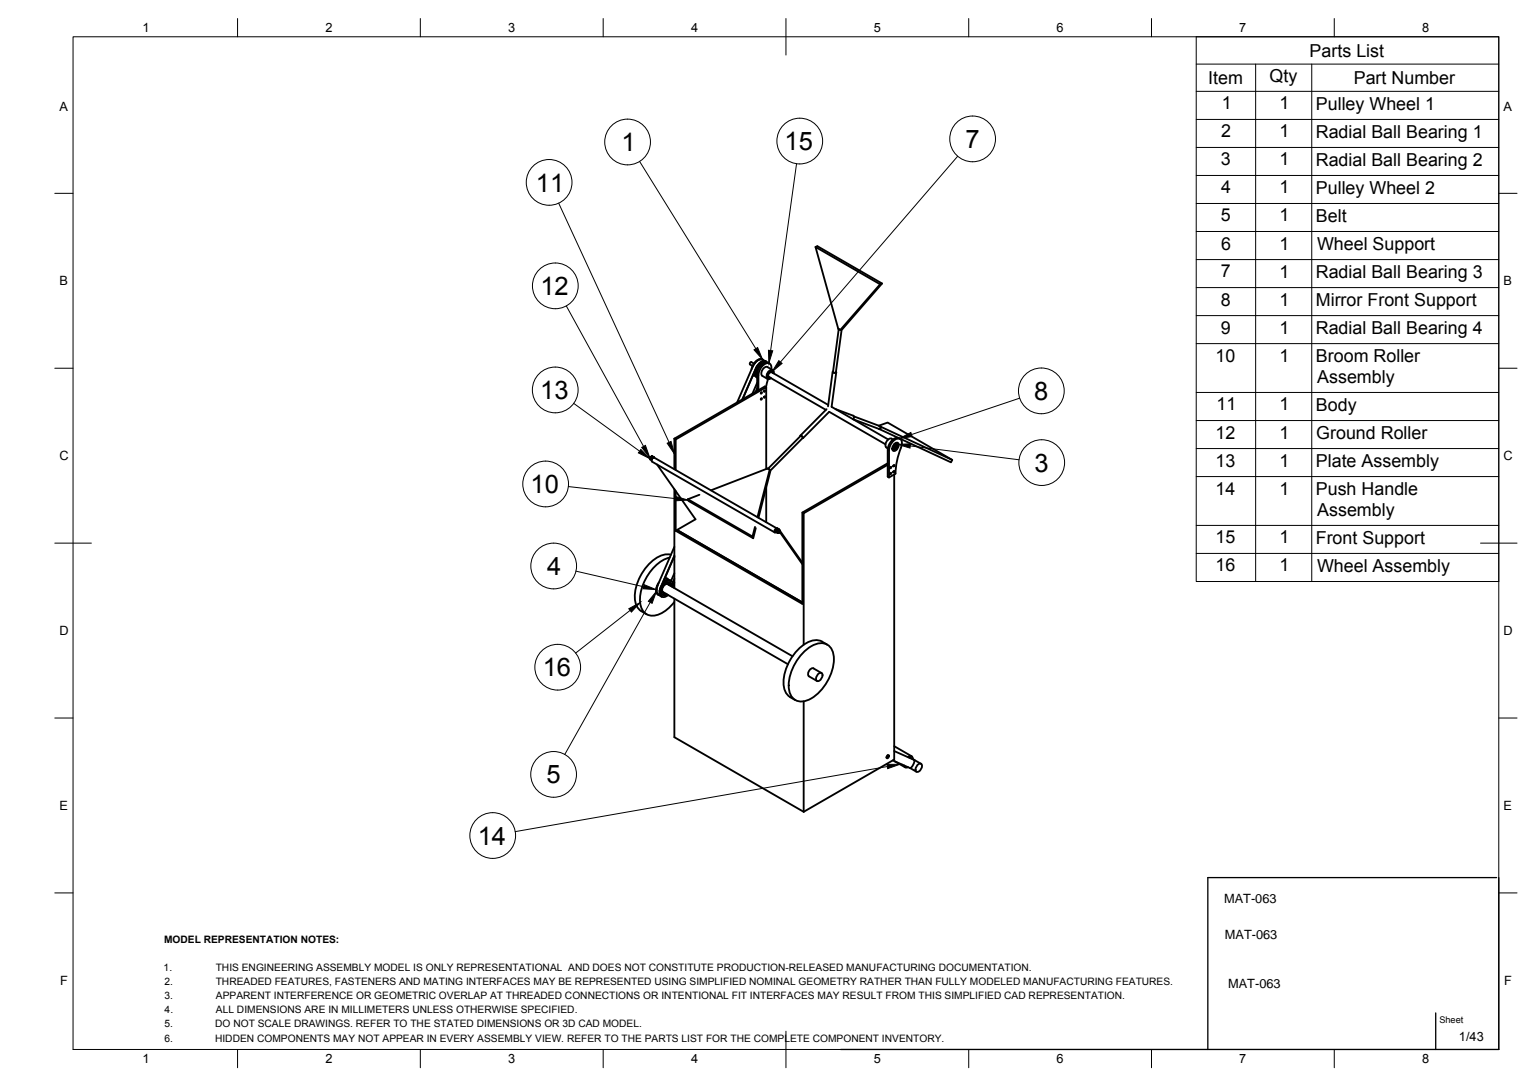
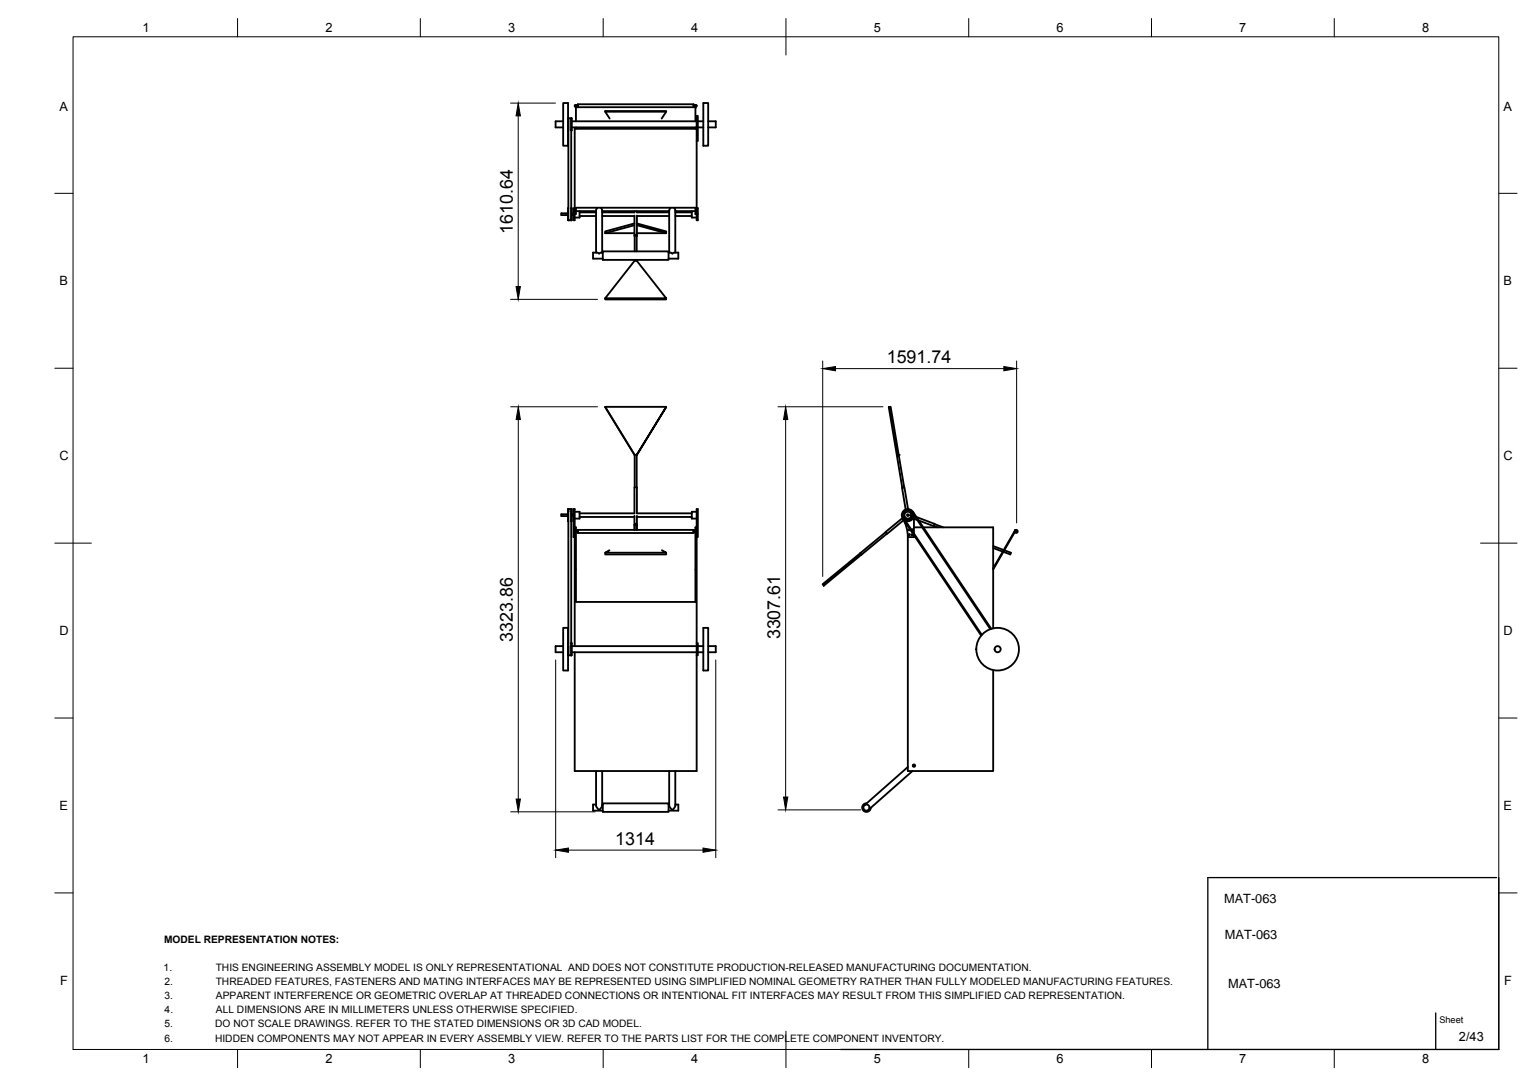
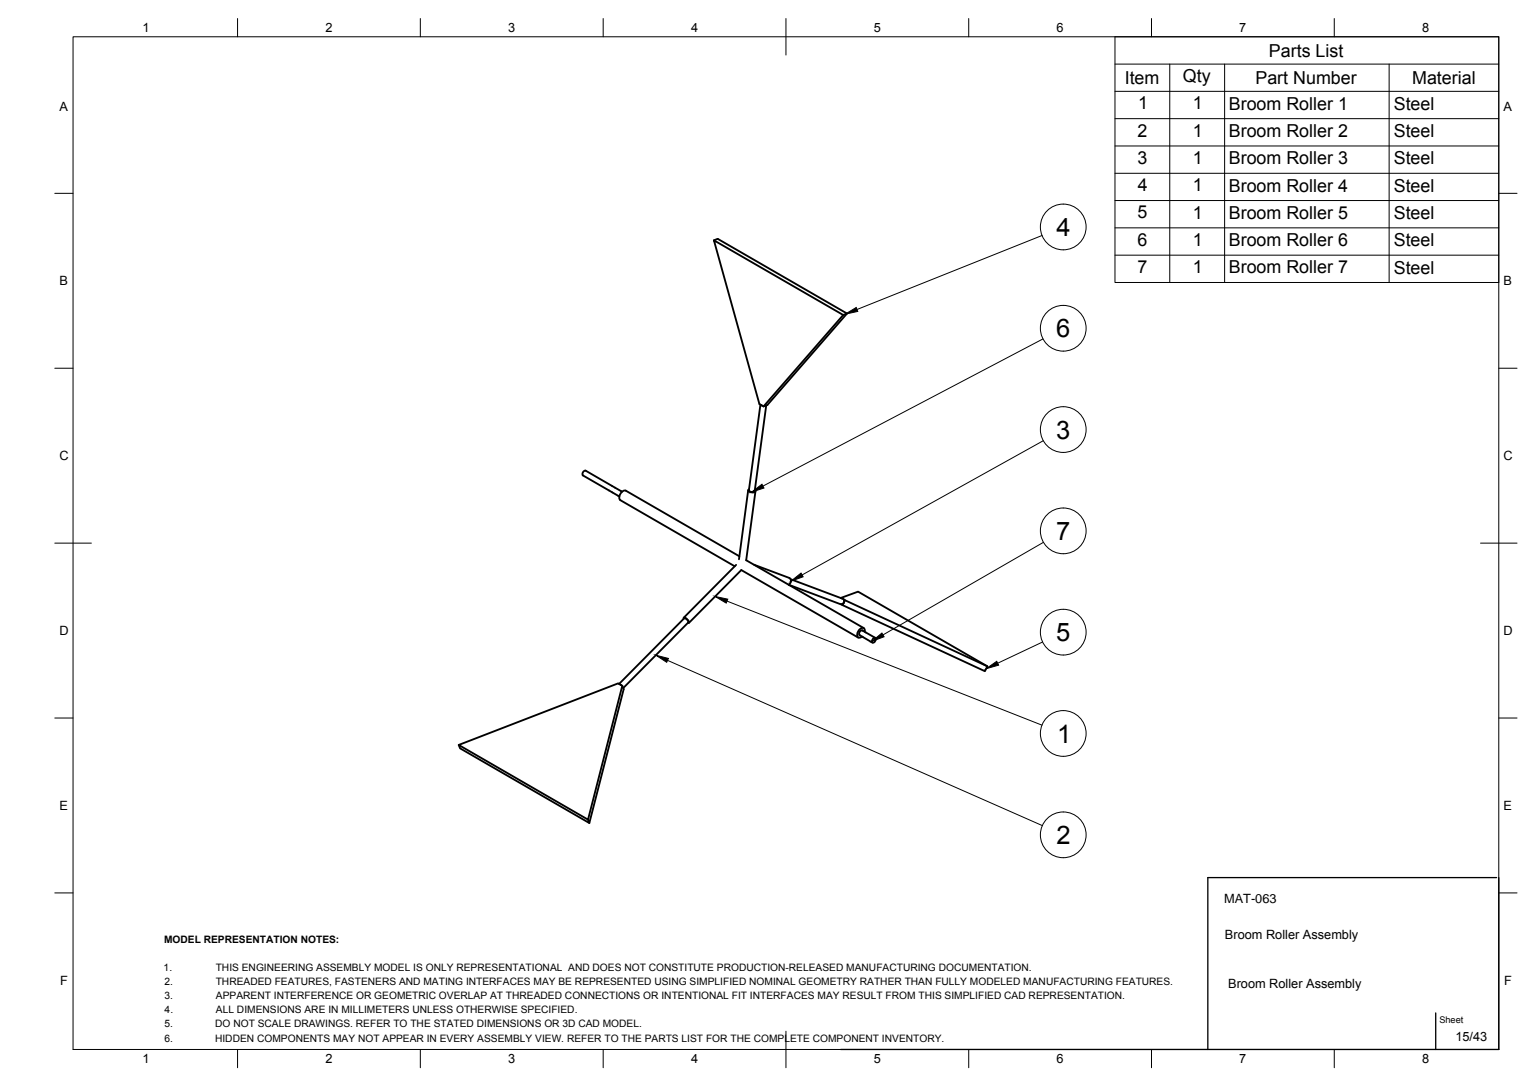
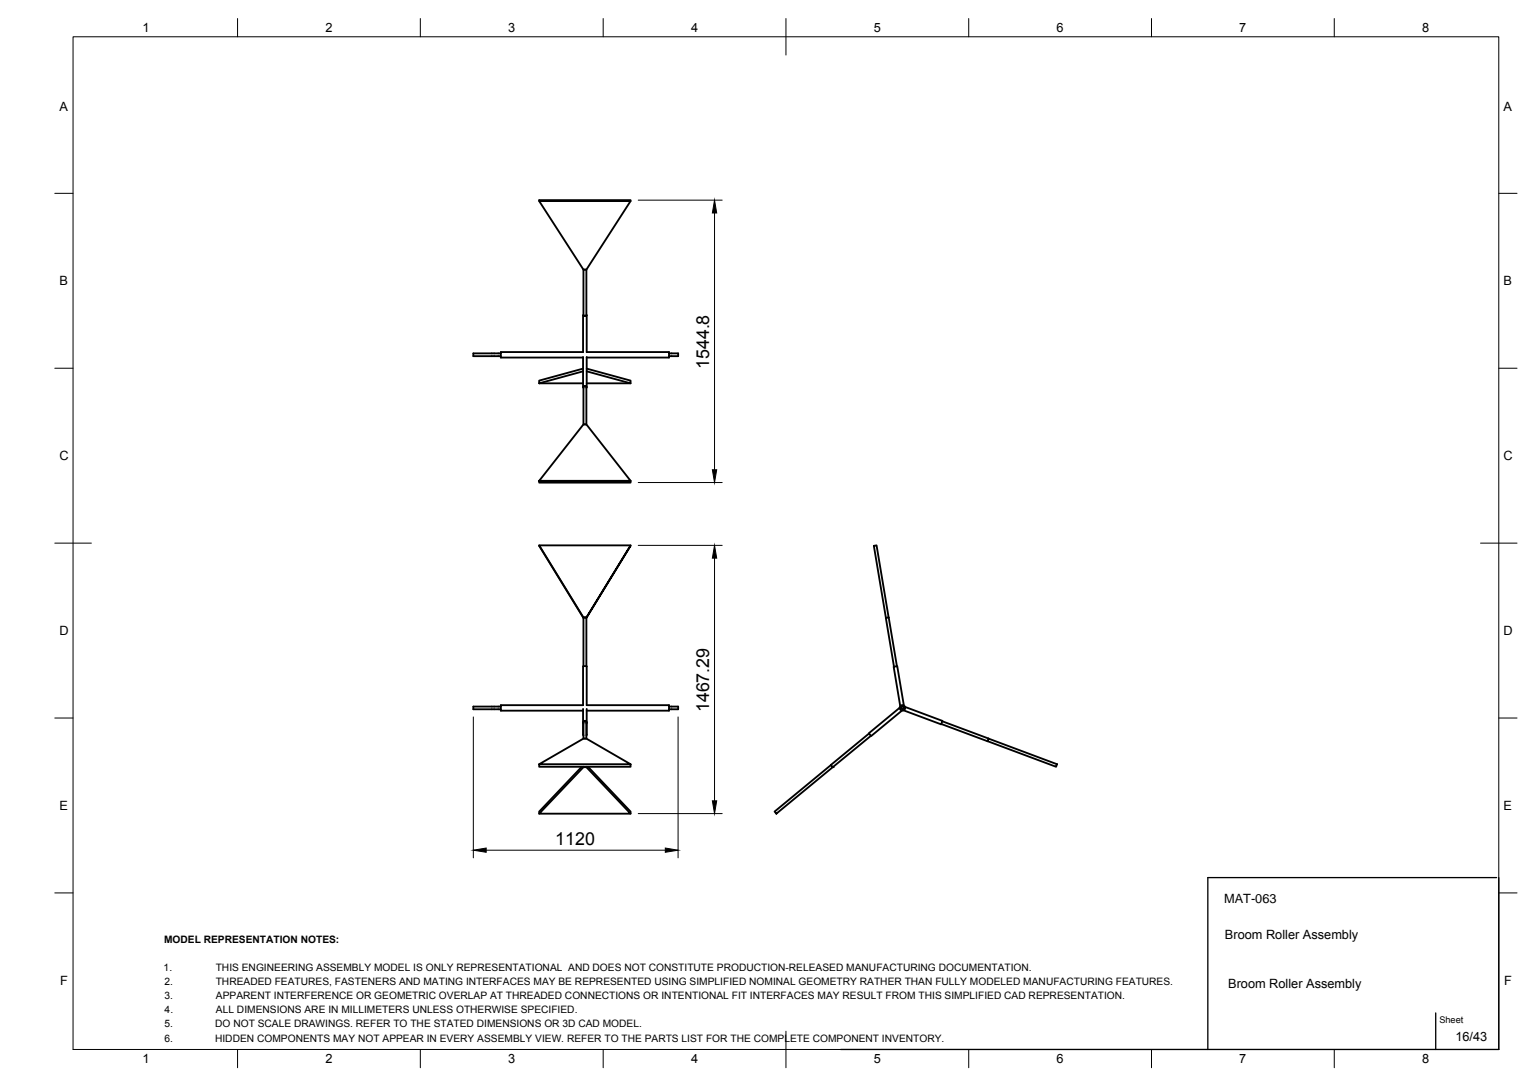
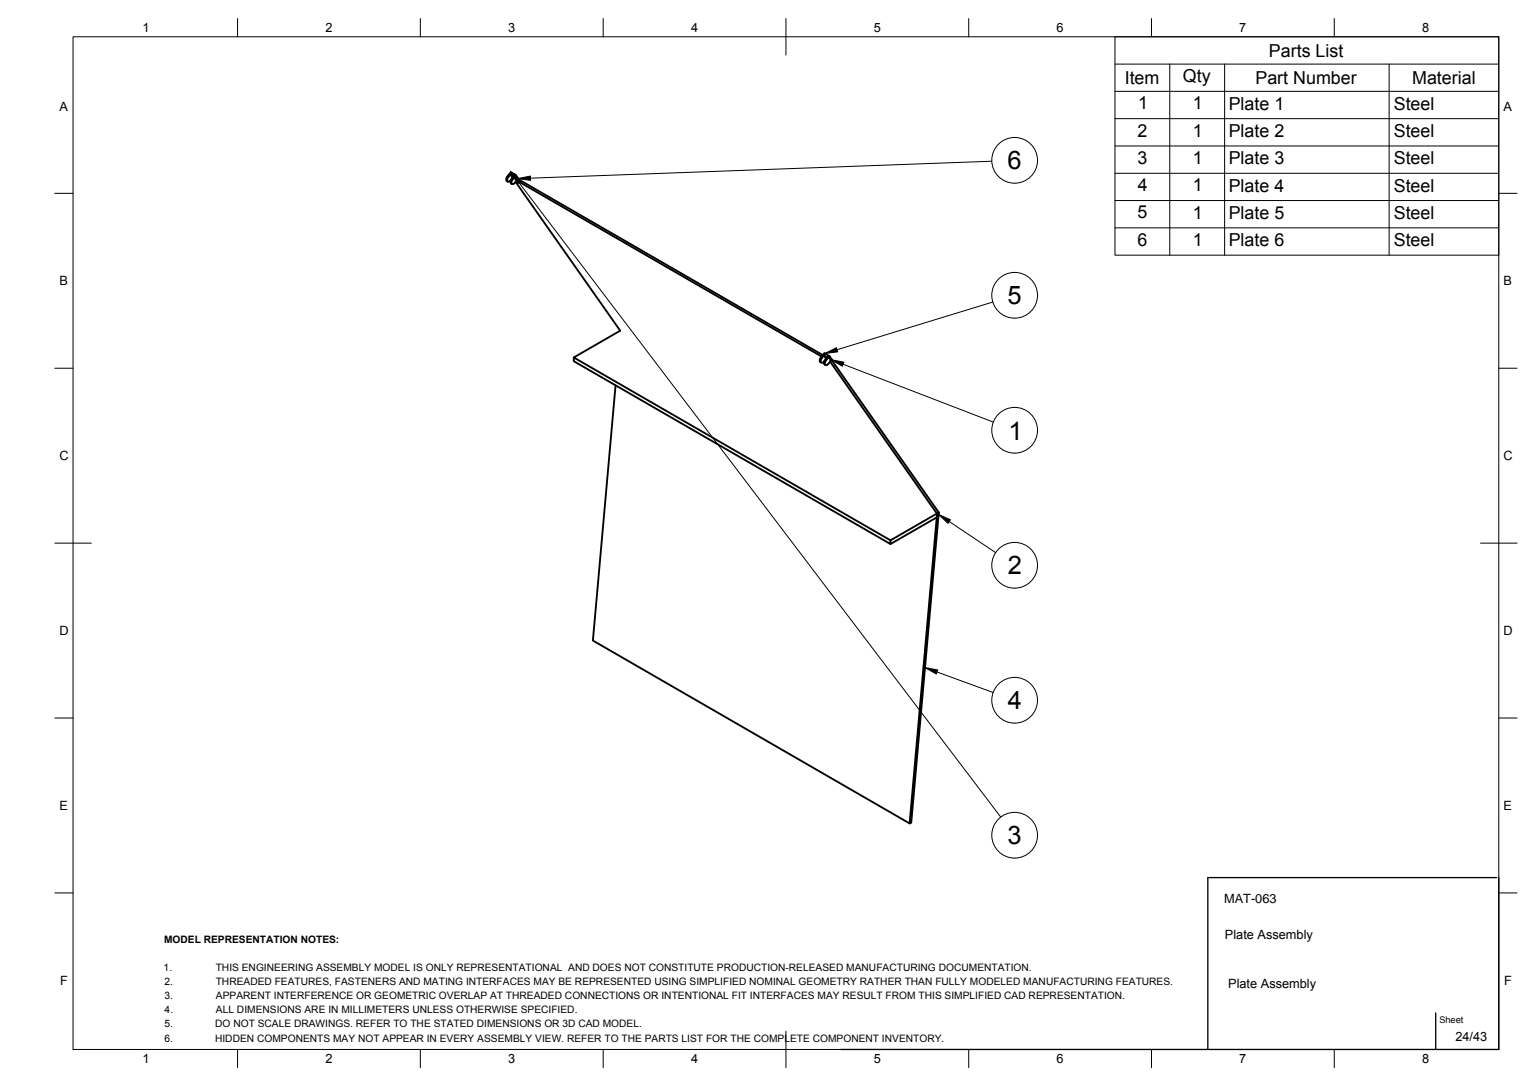
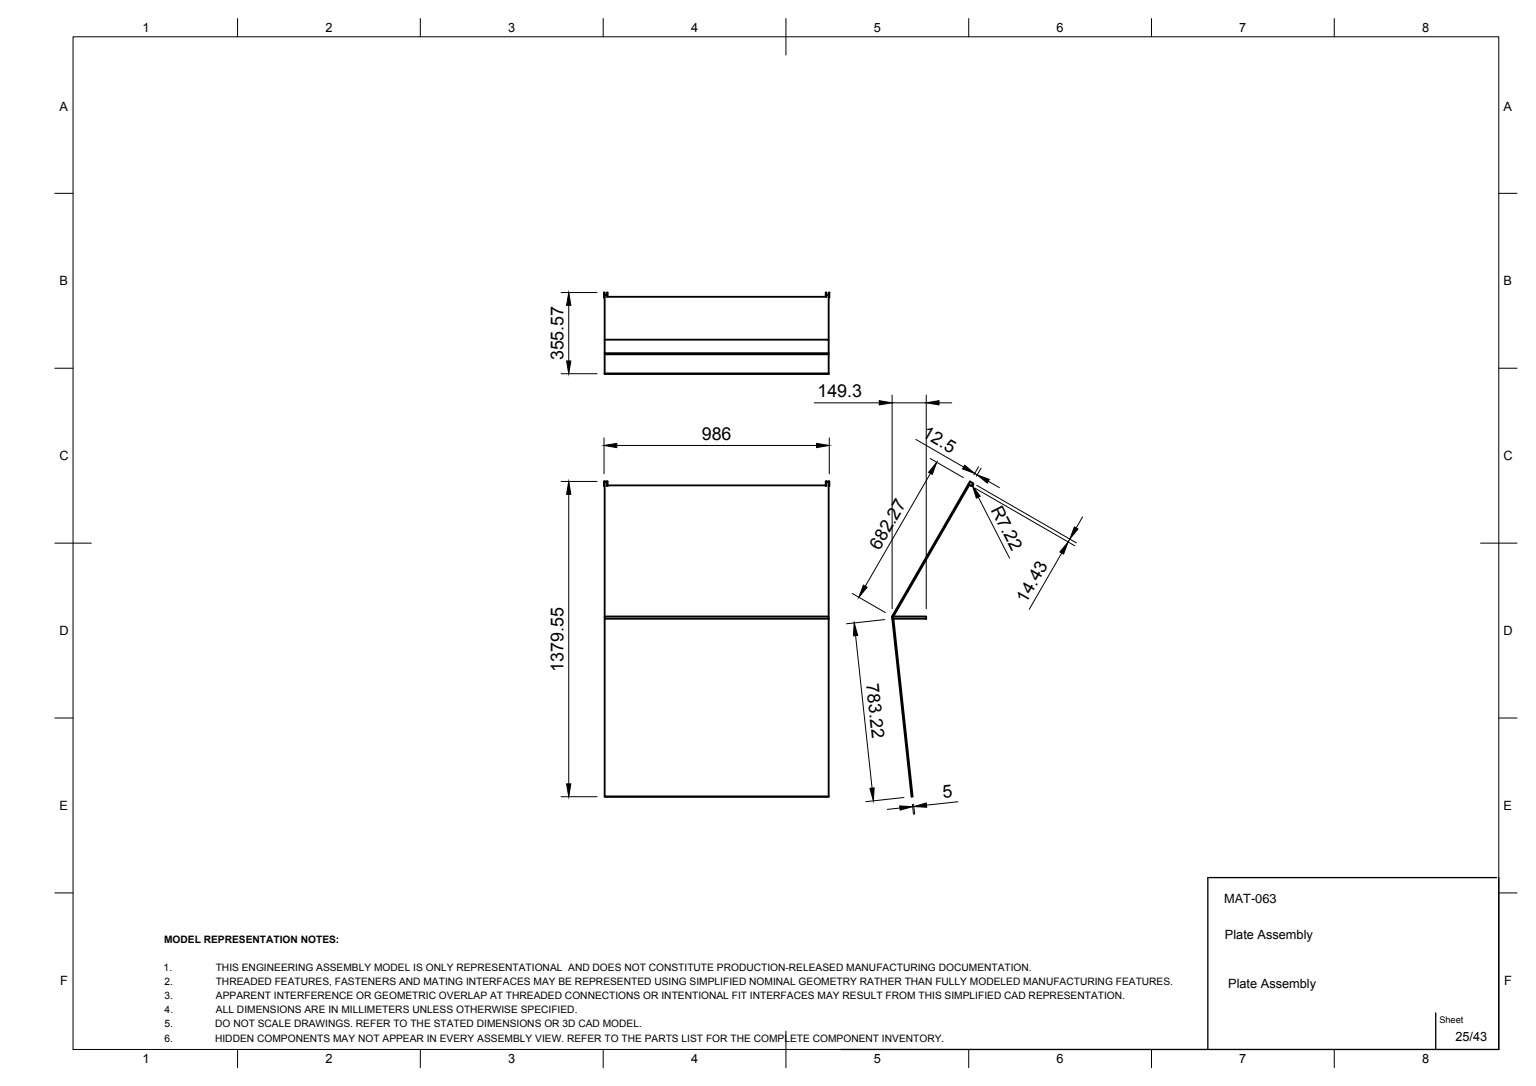
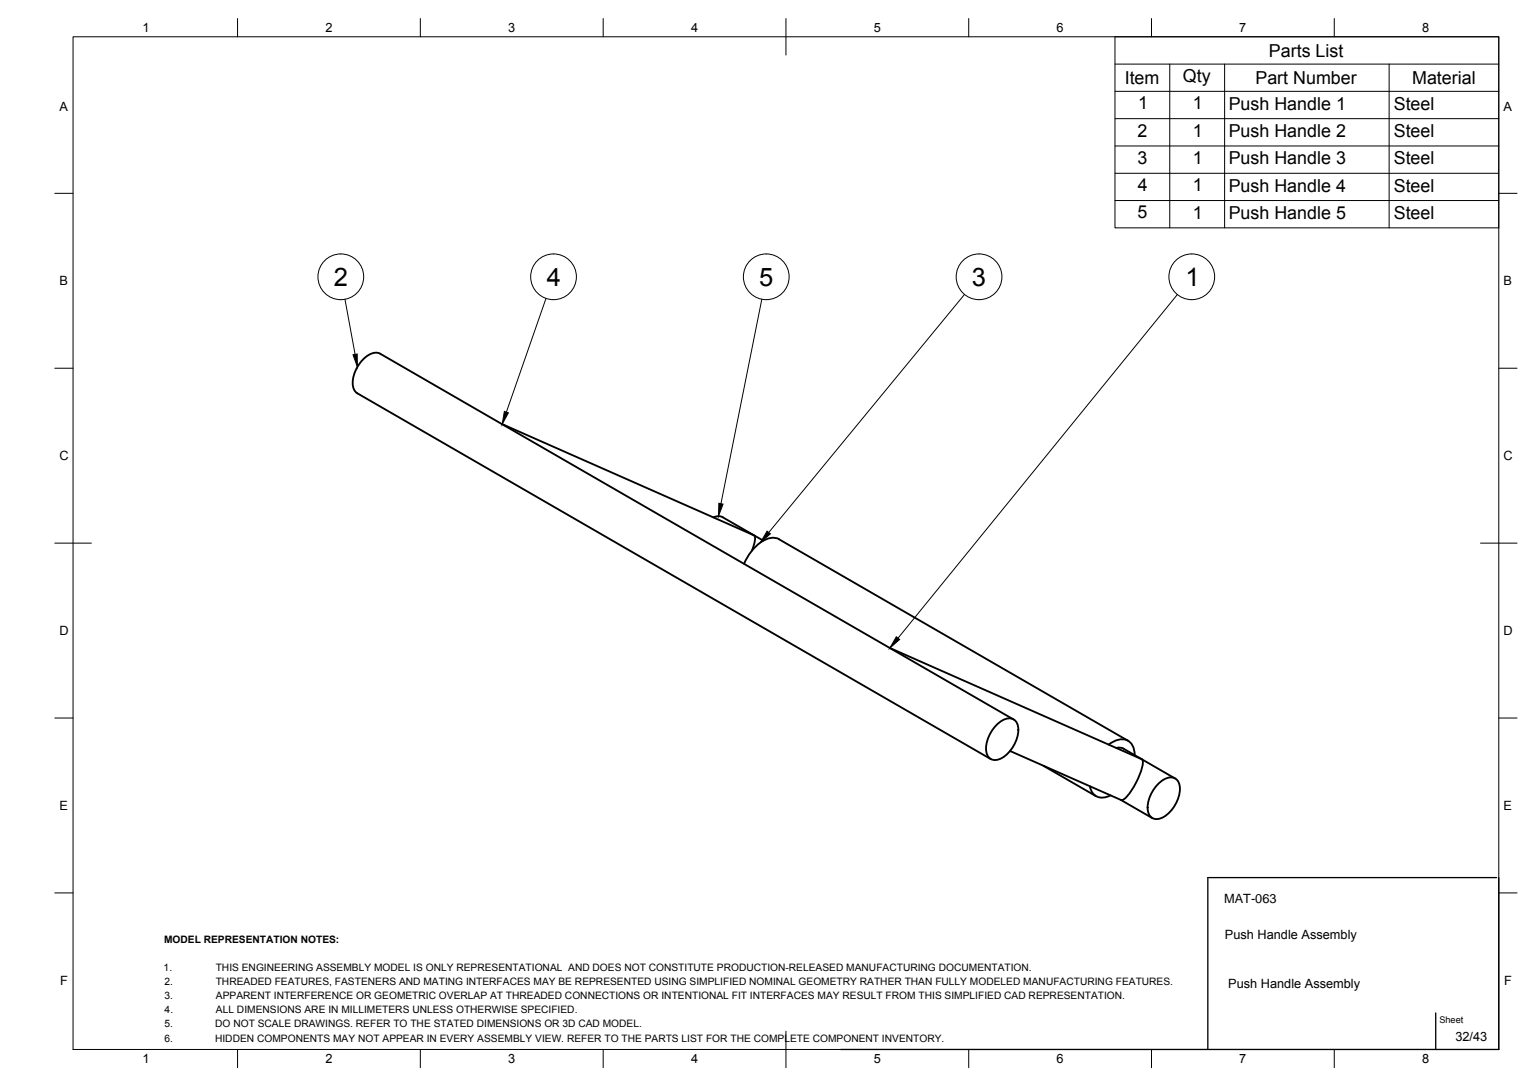
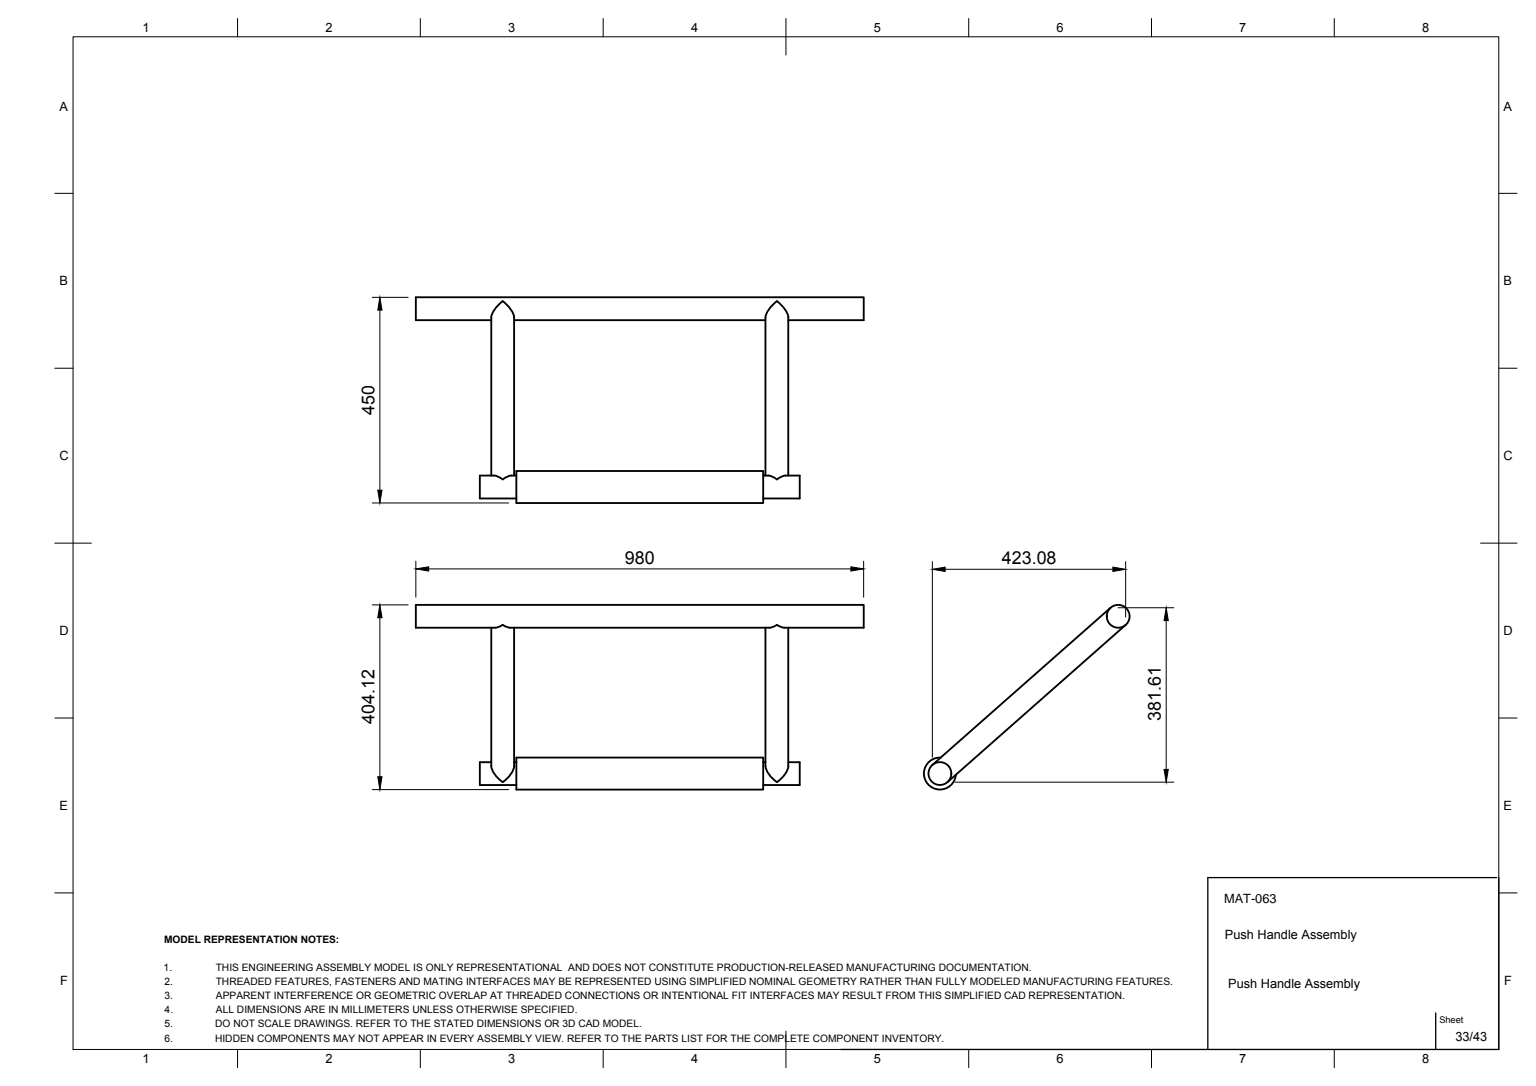
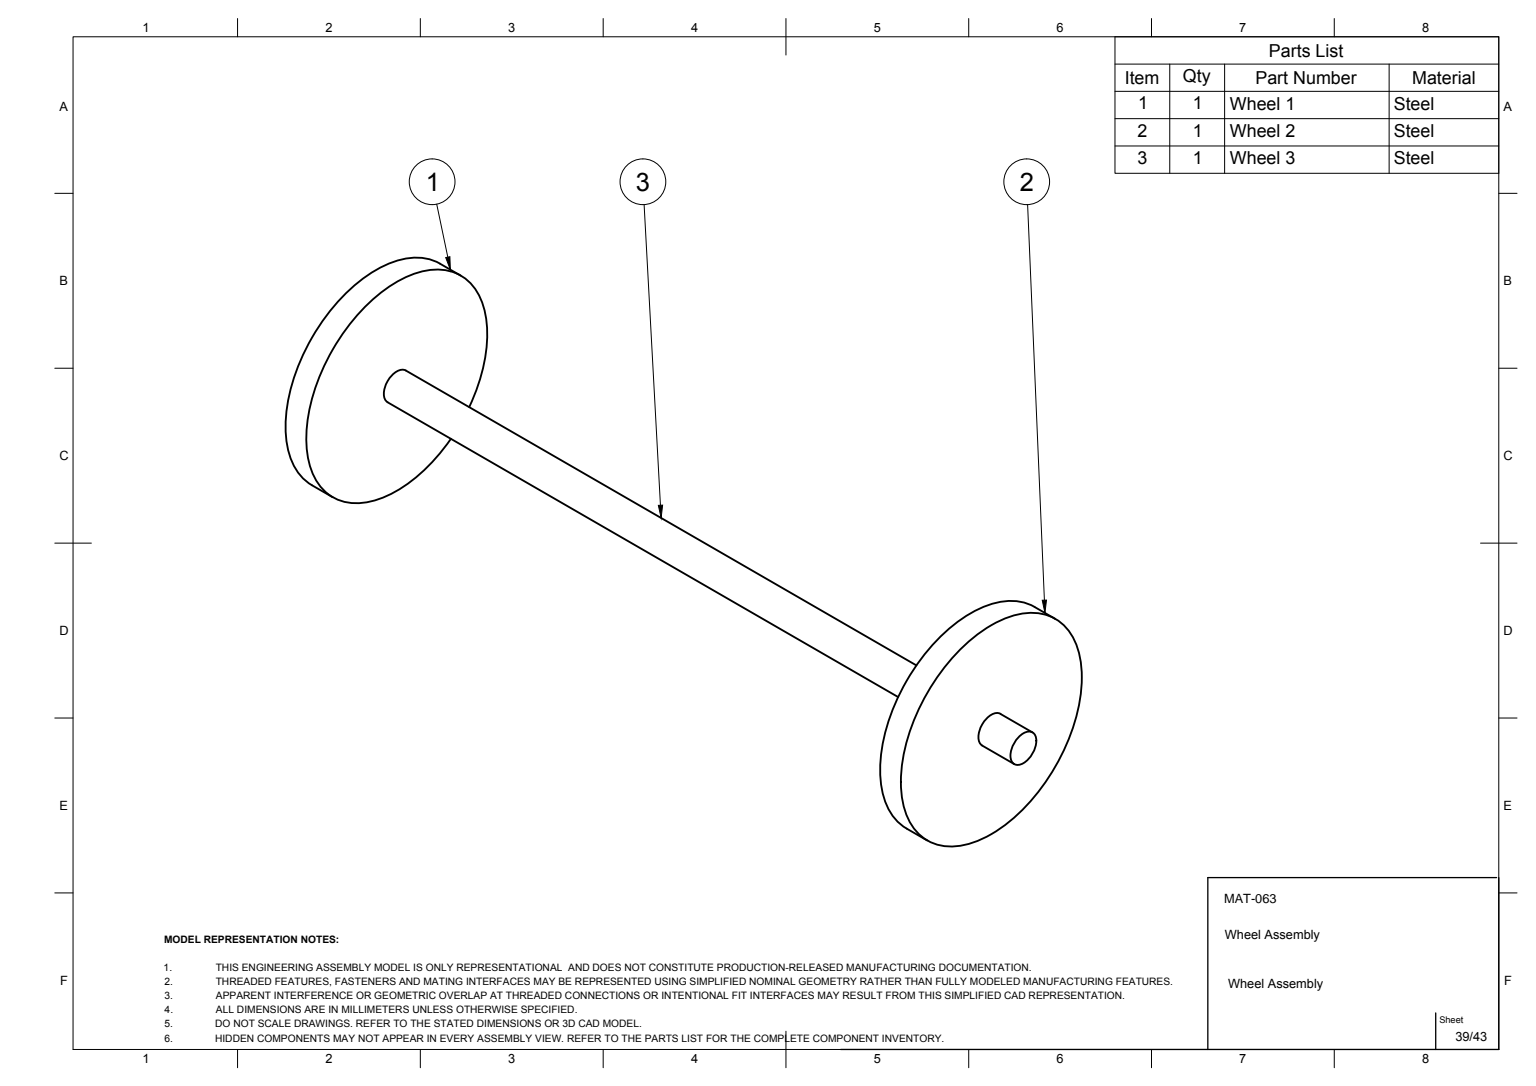
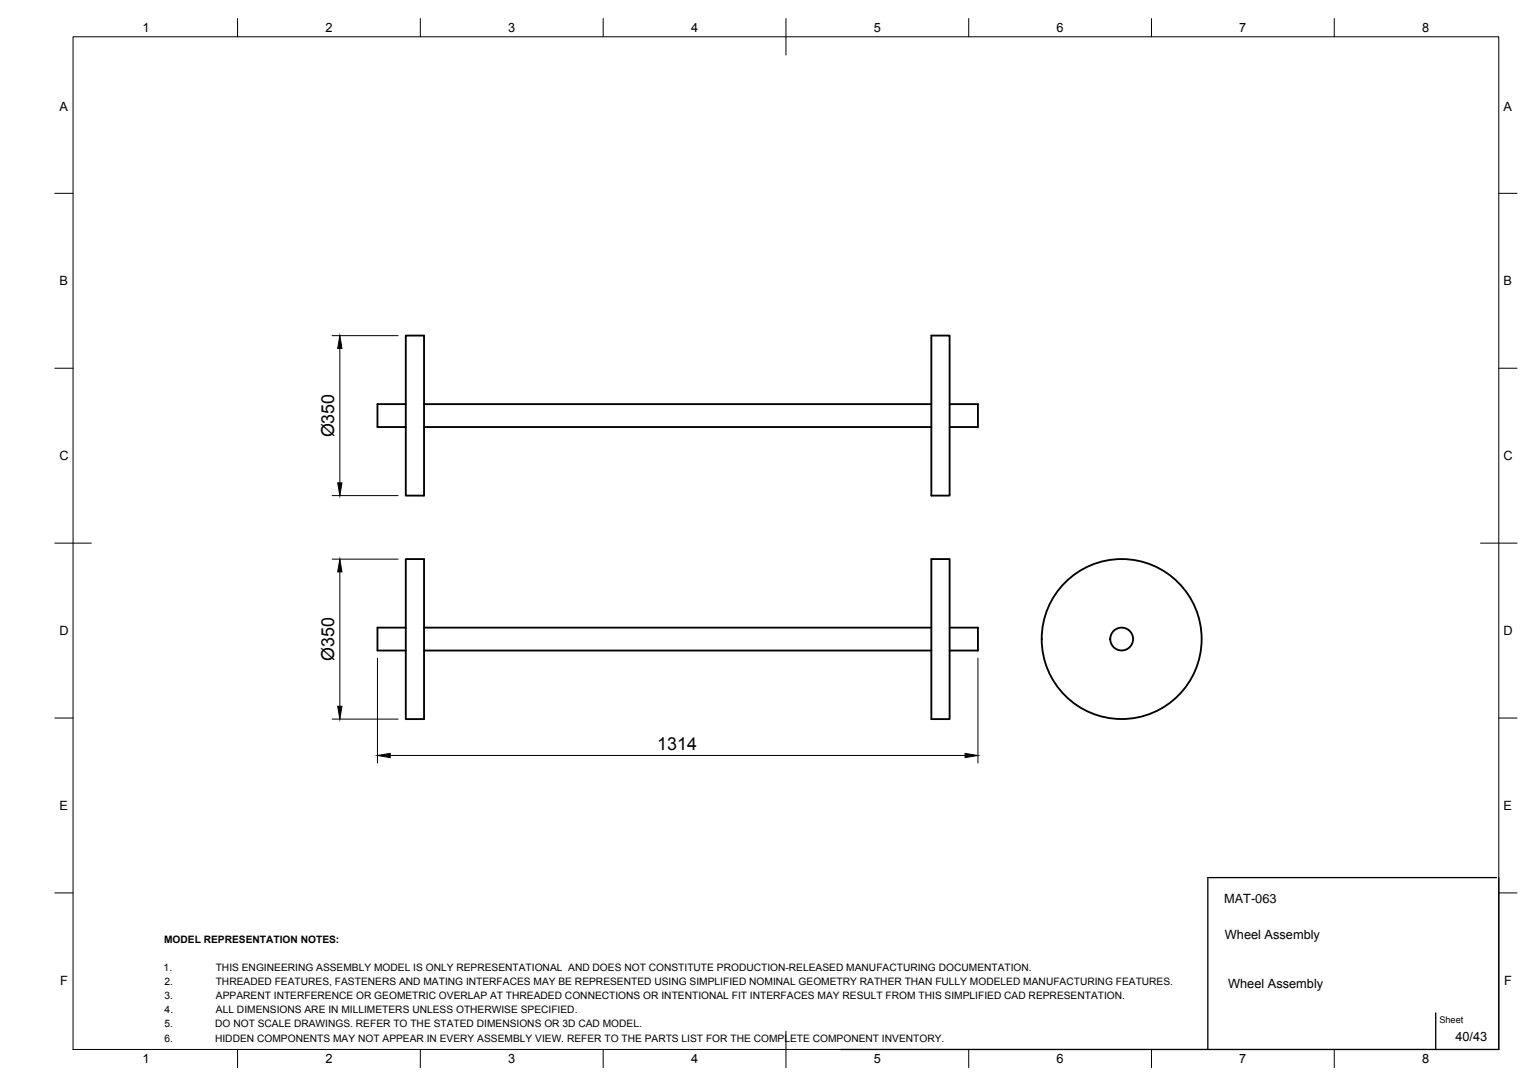
ISO-10303-21;
HEADER;
/* Generated by software containing ST-Developer
 * from STEP Tools, Inc. (www.steptools.com) 
 */

FILE_DESCRIPTION(
/* description */ (''),
/* implementation_level */ '2;1');

FILE_NAME(
/* name */ 'MAT-063',
/* time_stamp */ '2026-10-24T09:43:01-07:00',
/* author */ (''),
/* organization */ (''),
/* preprocessor_version */ 'ST-DEVELOPER v20.2',
/* originating_system */ 'Autodesk Translation Framework v15.15.0.0',
/* authorisation */ '');

FILE_SCHEMA (('AUTOMOTIVE_DESIGN { 1 0 10303 214 3 1 1 }'));
ENDSEC;

DATA;
#10=MECHANICAL_DESIGN_GEOMETRIC_PRESENTATION_REPRESENTATION('',(#273,#274,
#275,#276,#277,#278,#279,#280,#281,#282,#283,#284,#285,#286,#287,#288,#289,
#290,#291,#292,#293,#294,#295,#296,#297,#298,#299,#300,#301,#302,#303,#304,
#305),#11112);
#11=ELLIPSE('',#7146,0.035355338987388,0.0249999999491312);
#12=ELLIPSE('',#7147,0.0353553389873879,0.0249999999491312);
#13=ELLIPSE('',#7149,0.0353553389873867,0.0249999999491303);
#14=ELLIPSE('',#7150,0.0353553389873867,0.0249999999491303);
#15=ELLIPSE('',#7169,0.035355338987388,0.0249999999491312);
#16=ELLIPSE('',#7170,0.0353553389873879,0.0249999999491312);
#17=ELLIPSE('',#7172,0.0353553389873867,0.0249999999491303);
#18=ELLIPSE('',#7173,0.0353553389873867,0.0249999999491303);
#19=ITEM_DEFINED_TRANSFORMATION($,$,#6828,#6954);
#20=ITEM_DEFINED_TRANSFORMATION($,$,#6838,#6955);
#21=ITEM_DEFINED_TRANSFORMATION($,$,#6860,#6956);
#22=ITEM_DEFINED_TRANSFORMATION($,$,#6870,#6957);
#23=ITEM_DEFINED_TRANSFORMATION($,$,#6892,#6958);
#24=ITEM_DEFINED_TRANSFORMATION($,$,#6914,#6959);
#25=ITEM_DEFINED_TRANSFORMATION($,$,#6924,#6960);
#26=ITEM_DEFINED_TRANSFORMATION($,$,#7045,#7137);
#27=ITEM_DEFINED_TRANSFORMATION($,$,#7060,#7138);
#28=ITEM_DEFINED_TRANSFORMATION($,$,#7067,#7139);
#29=ITEM_DEFINED_TRANSFORMATION($,$,#7082,#7140);
#30=ITEM_DEFINED_TRANSFORMATION($,$,#7107,#7141);
#31=ITEM_DEFINED_TRANSFORMATION($,$,#7122,#7142);
#32=ITEM_DEFINED_TRANSFORMATION($,$,#7144,#7181);
#33=ITEM_DEFINED_TRANSFORMATION($,$,#7152,#7182);
#34=ITEM_DEFINED_TRANSFORMATION($,$,#7158,#7183);
#35=ITEM_DEFINED_TRANSFORMATION($,$,#7167,#7184);
#36=ITEM_DEFINED_TRANSFORMATION($,$,#7175,#7185);
#37=ITEM_DEFINED_TRANSFORMATION($,$,#7217,#7241);
#38=ITEM_DEFINED_TRANSFORMATION($,$,#7226,#7242);
#39=ITEM_DEFINED_TRANSFORMATION($,$,#7235,#7243);
#40=ITEM_DEFINED_TRANSFORMATION($,$,#6408,#7244);
#41=ITEM_DEFINED_TRANSFORMATION($,$,#6461,#7245);
#42=ITEM_DEFINED_TRANSFORMATION($,$,#6520,#7246);
#43=ITEM_DEFINED_TRANSFORMATION($,$,#6579,#7247);
#44=ITEM_DEFINED_TRANSFORMATION($,$,#6632,#7248);
#45=ITEM_DEFINED_TRANSFORMATION($,$,#6657,#7249);
#46=ITEM_DEFINED_TRANSFORMATION($,$,#6679,#7250);
#47=ITEM_DEFINED_TRANSFORMATION($,$,#6738,#7251);
#48=ITEM_DEFINED_TRANSFORMATION($,$,#6768,#7252);
#49=ITEM_DEFINED_TRANSFORMATION($,$,#6827,#7253);
#50=ITEM_DEFINED_TRANSFORMATION($,$,#6961,#7254);
#51=ITEM_DEFINED_TRANSFORMATION($,$,#7030,#7255);
#52=ITEM_DEFINED_TRANSFORMATION($,$,#7044,#7256);
#53=ITEM_DEFINED_TRANSFORMATION($,$,#7143,#7257);
#54=ITEM_DEFINED_TRANSFORMATION($,$,#7186,#7258);
#55=ITEM_DEFINED_TRANSFORMATION($,$,#7216,#7259);
#56=(
REPRESENTATION_RELATIONSHIP($,$,#11240,#11239)
REPRESENTATION_RELATIONSHIP_WITH_TRANSFORMATION(#19)
SHAPE_REPRESENTATION_RELATIONSHIP()
);
#57=(
REPRESENTATION_RELATIONSHIP($,$,#11241,#11239)
REPRESENTATION_RELATIONSHIP_WITH_TRANSFORMATION(#20)
SHAPE_REPRESENTATION_RELATIONSHIP()
);
#58=(
REPRESENTATION_RELATIONSHIP($,$,#11242,#11239)
REPRESENTATION_RELATIONSHIP_WITH_TRANSFORMATION(#21)
SHAPE_REPRESENTATION_RELATIONSHIP()
);
#59=(
REPRESENTATION_RELATIONSHIP($,$,#11243,#11239)
REPRESENTATION_RELATIONSHIP_WITH_TRANSFORMATION(#22)
SHAPE_REPRESENTATION_RELATIONSHIP()
);
#60=(
REPRESENTATION_RELATIONSHIP($,$,#11244,#11239)
REPRESENTATION_RELATIONSHIP_WITH_TRANSFORMATION(#23)
SHAPE_REPRESENTATION_RELATIONSHIP()
);
#61=(
REPRESENTATION_RELATIONSHIP($,$,#11245,#11239)
REPRESENTATION_RELATIONSHIP_WITH_TRANSFORMATION(#24)
SHAPE_REPRESENTATION_RELATIONSHIP()
);
#62=(
REPRESENTATION_RELATIONSHIP($,$,#11246,#11239)
REPRESENTATION_RELATIONSHIP_WITH_TRANSFORMATION(#25)
SHAPE_REPRESENTATION_RELATIONSHIP()
);
#63=(
REPRESENTATION_RELATIONSHIP($,$,#11250,#11249)
REPRESENTATION_RELATIONSHIP_WITH_TRANSFORMATION(#26)
SHAPE_REPRESENTATION_RELATIONSHIP()
);
#64=(
REPRESENTATION_RELATIONSHIP($,$,#11251,#11249)
REPRESENTATION_RELATIONSHIP_WITH_TRANSFORMATION(#27)
SHAPE_REPRESENTATION_RELATIONSHIP()
);
#65=(
REPRESENTATION_RELATIONSHIP($,$,#11252,#11249)
REPRESENTATION_RELATIONSHIP_WITH_TRANSFORMATION(#28)
SHAPE_REPRESENTATION_RELATIONSHIP()
);
#66=(
REPRESENTATION_RELATIONSHIP($,$,#11253,#11249)
REPRESENTATION_RELATIONSHIP_WITH_TRANSFORMATION(#29)
SHAPE_REPRESENTATION_RELATIONSHIP()
);
#67=(
REPRESENTATION_RELATIONSHIP($,$,#11254,#11249)
REPRESENTATION_RELATIONSHIP_WITH_TRANSFORMATION(#30)
SHAPE_REPRESENTATION_RELATIONSHIP()
);
#68=(
REPRESENTATION_RELATIONSHIP($,$,#11255,#11249)
REPRESENTATION_RELATIONSHIP_WITH_TRANSFORMATION(#31)
SHAPE_REPRESENTATION_RELATIONSHIP()
);
#69=(
REPRESENTATION_RELATIONSHIP($,$,#11257,#11256)
REPRESENTATION_RELATIONSHIP_WITH_TRANSFORMATION(#32)
SHAPE_REPRESENTATION_RELATIONSHIP()
);
#70=(
REPRESENTATION_RELATIONSHIP($,$,#11258,#11256)
REPRESENTATION_RELATIONSHIP_WITH_TRANSFORMATION(#33)
SHAPE_REPRESENTATION_RELATIONSHIP()
);
#71=(
REPRESENTATION_RELATIONSHIP($,$,#11259,#11256)
REPRESENTATION_RELATIONSHIP_WITH_TRANSFORMATION(#34)
SHAPE_REPRESENTATION_RELATIONSHIP()
);
#72=(
REPRESENTATION_RELATIONSHIP($,$,#11260,#11256)
REPRESENTATION_RELATIONSHIP_WITH_TRANSFORMATION(#35)
SHAPE_REPRESENTATION_RELATIONSHIP()
);
#73=(
REPRESENTATION_RELATIONSHIP($,$,#11261,#11256)
REPRESENTATION_RELATIONSHIP_WITH_TRANSFORMATION(#36)
SHAPE_REPRESENTATION_RELATIONSHIP()
);
#74=(
REPRESENTATION_RELATIONSHIP($,$,#11264,#11263)
REPRESENTATION_RELATIONSHIP_WITH_TRANSFORMATION(#37)
SHAPE_REPRESENTATION_RELATIONSHIP()
);
#75=(
REPRESENTATION_RELATIONSHIP($,$,#11265,#11263)
REPRESENTATION_RELATIONSHIP_WITH_TRANSFORMATION(#38)
SHAPE_REPRESENTATION_RELATIONSHIP()
);
#76=(
REPRESENTATION_RELATIONSHIP($,$,#11266,#11263)
REPRESENTATION_RELATIONSHIP_WITH_TRANSFORMATION(#39)
SHAPE_REPRESENTATION_RELATIONSHIP()
);
#77=(
REPRESENTATION_RELATIONSHIP($,$,#11230,#11229)
REPRESENTATION_RELATIONSHIP_WITH_TRANSFORMATION(#40)
SHAPE_REPRESENTATION_RELATIONSHIP()
);
#78=(
REPRESENTATION_RELATIONSHIP($,$,#11231,#11229)
REPRESENTATION_RELATIONSHIP_WITH_TRANSFORMATION(#41)
SHAPE_REPRESENTATION_RELATIONSHIP()
);
#79=(
REPRESENTATION_RELATIONSHIP($,$,#11232,#11229)
REPRESENTATION_RELATIONSHIP_WITH_TRANSFORMATION(#42)
SHAPE_REPRESENTATION_RELATIONSHIP()
);
#80=(
REPRESENTATION_RELATIONSHIP($,$,#11233,#11229)
REPRESENTATION_RELATIONSHIP_WITH_TRANSFORMATION(#43)
SHAPE_REPRESENTATION_RELATIONSHIP()
);
#81=(
REPRESENTATION_RELATIONSHIP($,$,#11234,#11229)
REPRESENTATION_RELATIONSHIP_WITH_TRANSFORMATION(#44)
SHAPE_REPRESENTATION_RELATIONSHIP()
);
#82=(
REPRESENTATION_RELATIONSHIP($,$,#11235,#11229)
REPRESENTATION_RELATIONSHIP_WITH_TRANSFORMATION(#45)
SHAPE_REPRESENTATION_RELATIONSHIP()
);
#83=(
REPRESENTATION_RELATIONSHIP($,$,#11236,#11229)
REPRESENTATION_RELATIONSHIP_WITH_TRANSFORMATION(#46)
SHAPE_REPRESENTATION_RELATIONSHIP()
);
#84=(
REPRESENTATION_RELATIONSHIP($,$,#11237,#11229)
REPRESENTATION_RELATIONSHIP_WITH_TRANSFORMATION(#47)
SHAPE_REPRESENTATION_RELATIONSHIP()
);
#85=(
REPRESENTATION_RELATIONSHIP($,$,#11238,#11229)
REPRESENTATION_RELATIONSHIP_WITH_TRANSFORMATION(#48)
SHAPE_REPRESENTATION_RELATIONSHIP()
);
#86=(
REPRESENTATION_RELATIONSHIP($,$,#11239,#11229)
REPRESENTATION_RELATIONSHIP_WITH_TRANSFORMATION(#49)
SHAPE_REPRESENTATION_RELATIONSHIP()
);
#87=(
REPRESENTATION_RELATIONSHIP($,$,#11247,#11229)
REPRESENTATION_RELATIONSHIP_WITH_TRANSFORMATION(#50)
SHAPE_REPRESENTATION_RELATIONSHIP()
);
#88=(
REPRESENTATION_RELATIONSHIP($,$,#11248,#11229)
REPRESENTATION_RELATIONSHIP_WITH_TRANSFORMATION(#51)
SHAPE_REPRESENTATION_RELATIONSHIP()
);
#89=(
REPRESENTATION_RELATIONSHIP($,$,#11249,#11229)
REPRESENTATION_RELATIONSHIP_WITH_TRANSFORMATION(#52)
SHAPE_REPRESENTATION_RELATIONSHIP()
);
#90=(
REPRESENTATION_RELATIONSHIP($,$,#11256,#11229)
REPRESENTATION_RELATIONSHIP_WITH_TRANSFORMATION(#53)
SHAPE_REPRESENTATION_RELATIONSHIP()
);
#91=(
REPRESENTATION_RELATIONSHIP($,$,#11262,#11229)
REPRESENTATION_RELATIONSHIP_WITH_TRANSFORMATION(#54)
SHAPE_REPRESENTATION_RELATIONSHIP()
);
#92=(
REPRESENTATION_RELATIONSHIP($,$,#11263,#11229)
REPRESENTATION_RELATIONSHIP_WITH_TRANSFORMATION(#55)
SHAPE_REPRESENTATION_RELATIONSHIP()
);
#93=CONTEXT_DEPENDENT_SHAPE_REPRESENTATION(#56,#11172);
#94=CONTEXT_DEPENDENT_SHAPE_REPRESENTATION(#57,#11173);
#95=CONTEXT_DEPENDENT_SHAPE_REPRESENTATION(#58,#11174);
#96=CONTEXT_DEPENDENT_SHAPE_REPRESENTATION(#59,#11175);
#97=CONTEXT_DEPENDENT_SHAPE_REPRESENTATION(#60,#11176);
#98=CONTEXT_DEPENDENT_SHAPE_REPRESENTATION(#61,#11177);
#99=CONTEXT_DEPENDENT_SHAPE_REPRESENTATION(#62,#11178);
#100=CONTEXT_DEPENDENT_SHAPE_REPRESENTATION(#63,#11188);
#101=CONTEXT_DEPENDENT_SHAPE_REPRESENTATION(#64,#11189);
#102=CONTEXT_DEPENDENT_SHAPE_REPRESENTATION(#65,#11190);
#103=CONTEXT_DEPENDENT_SHAPE_REPRESENTATION(#66,#11191);
#104=CONTEXT_DEPENDENT_SHAPE_REPRESENTATION(#67,#11192);
#105=CONTEXT_DEPENDENT_SHAPE_REPRESENTATION(#68,#11193);
#106=CONTEXT_DEPENDENT_SHAPE_REPRESENTATION(#69,#11200);
#107=CONTEXT_DEPENDENT_SHAPE_REPRESENTATION(#70,#11201);
#108=CONTEXT_DEPENDENT_SHAPE_REPRESENTATION(#71,#11202);
#109=CONTEXT_DEPENDENT_SHAPE_REPRESENTATION(#72,#11203);
#110=CONTEXT_DEPENDENT_SHAPE_REPRESENTATION(#73,#11204);
#111=CONTEXT_DEPENDENT_SHAPE_REPRESENTATION(#74,#11210);
#112=CONTEXT_DEPENDENT_SHAPE_REPRESENTATION(#75,#11211);
#113=CONTEXT_DEPENDENT_SHAPE_REPRESENTATION(#76,#11212);
#114=CONTEXT_DEPENDENT_SHAPE_REPRESENTATION(#77,#11213);
#115=CONTEXT_DEPENDENT_SHAPE_REPRESENTATION(#78,#11214);
#116=CONTEXT_DEPENDENT_SHAPE_REPRESENTATION(#79,#11215);
#117=CONTEXT_DEPENDENT_SHAPE_REPRESENTATION(#80,#11216);
#118=CONTEXT_DEPENDENT_SHAPE_REPRESENTATION(#81,#11217);
#119=CONTEXT_DEPENDENT_SHAPE_REPRESENTATION(#82,#11218);
#120=CONTEXT_DEPENDENT_SHAPE_REPRESENTATION(#83,#11219);
#121=CONTEXT_DEPENDENT_SHAPE_REPRESENTATION(#84,#11220);
#122=CONTEXT_DEPENDENT_SHAPE_REPRESENTATION(#85,#11221);
#123=CONTEXT_DEPENDENT_SHAPE_REPRESENTATION(#86,#11222);
#124=CONTEXT_DEPENDENT_SHAPE_REPRESENTATION(#87,#11223);
#125=CONTEXT_DEPENDENT_SHAPE_REPRESENTATION(#88,#11224);
#126=CONTEXT_DEPENDENT_SHAPE_REPRESENTATION(#89,#11225);
#127=CONTEXT_DEPENDENT_SHAPE_REPRESENTATION(#90,#11226);
#128=CONTEXT_DEPENDENT_SHAPE_REPRESENTATION(#91,#11227);
#129=CONTEXT_DEPENDENT_SHAPE_REPRESENTATION(#92,#11228);
#130=NEXT_ASSEMBLY_USAGE_OCCURRENCE('Broom Roller 1:1',
'Broom Roller 1:1','Broom Roller 1:1',#11278,#11279,'Broom Roller 1:1');
#131=NEXT_ASSEMBLY_USAGE_OCCURRENCE('Broom Roller 2:1',
'Broom Roller 2:1','Broom Roller 2:1',#11278,#11280,'Broom Roller 2:1');
#132=NEXT_ASSEMBLY_USAGE_OCCURRENCE('Broom Roller 3:1',
'Broom Roller 3:1','Broom Roller 3:1',#11278,#11281,'Broom Roller 3:1');
#133=NEXT_ASSEMBLY_USAGE_OCCURRENCE('Broom Roller 4:1',
'Broom Roller 4:1','Broom Roller 4:1',#11278,#11282,'Broom Roller 4:1');
#134=NEXT_ASSEMBLY_USAGE_OCCURRENCE('Broom Roller 5:1',
'Broom Roller 5:1','Broom Roller 5:1',#11278,#11283,'Broom Roller 5:1');
#135=NEXT_ASSEMBLY_USAGE_OCCURRENCE('Broom Roller 6:1',
'Broom Roller 6:1','Broom Roller 6:1',#11278,#11284,'Broom Roller 6:1');
#136=NEXT_ASSEMBLY_USAGE_OCCURRENCE('Broom Roller 7:1',
'Broom Roller 7:1','Broom Roller 7:1',#11278,#11285,'Broom Roller 7:1');
#137=NEXT_ASSEMBLY_USAGE_OCCURRENCE('Plate 1:1','Plate 1:1','Plate 1:1',
#11288,#11289,'Plate 1:1');
#138=NEXT_ASSEMBLY_USAGE_OCCURRENCE('Plate 2:1','Plate 2:1','Plate 2:1',
#11288,#11290,'Plate 2:1');
#139=NEXT_ASSEMBLY_USAGE_OCCURRENCE('Plate 3:1','Plate 3:1','Plate 3:1',
#11288,#11291,'Plate 3:1');
#140=NEXT_ASSEMBLY_USAGE_OCCURRENCE('Plate 4:1','Plate 4:1','Plate 4:1',
#11288,#11292,'Plate 4:1');
#141=NEXT_ASSEMBLY_USAGE_OCCURRENCE('Plate 5:1','Plate 5:1','Plate 5:1',
#11288,#11293,'Plate 5:1');
#142=NEXT_ASSEMBLY_USAGE_OCCURRENCE('Plate 6:1','Plate 6:1','Plate 6:1',
#11288,#11294,'Plate 6:1');
#143=NEXT_ASSEMBLY_USAGE_OCCURRENCE('Push Handle 1:1','Push Handle 1:1',
'Push Handle 1:1',#11295,#11296,'Push Handle 1:1');
#144=NEXT_ASSEMBLY_USAGE_OCCURRENCE('Push Handle 2:1','Push Handle 2:1',
'Push Handle 2:1',#11295,#11297,'Push Handle 2:1');
#145=NEXT_ASSEMBLY_USAGE_OCCURRENCE('Push Handle 3:1','Push Handle 3:1',
'Push Handle 3:1',#11295,#11298,'Push Handle 3:1');
#146=NEXT_ASSEMBLY_USAGE_OCCURRENCE('Push Handle 4:1','Push Handle 4:1',
'Push Handle 4:1',#11295,#11299,'Push Handle 4:1');
#147=NEXT_ASSEMBLY_USAGE_OCCURRENCE('Push Handle 5:1','Push Handle 5:1',
'Push Handle 5:1',#11295,#11300,'Push Handle 5:1');
#148=NEXT_ASSEMBLY_USAGE_OCCURRENCE('Wheel 1:1','Wheel 1:1','Wheel 1:1',
#11302,#11303,'Wheel 1:1');
#149=NEXT_ASSEMBLY_USAGE_OCCURRENCE('Wheel 2:1','Wheel 2:1','Wheel 2:1',
#11302,#11304,'Wheel 2:1');
#150=NEXT_ASSEMBLY_USAGE_OCCURRENCE('Wheel 3:1','Wheel 3:1','Wheel 3:1',
#11302,#11305,'Wheel 3:1');
#151=NEXT_ASSEMBLY_USAGE_OCCURRENCE('Pulley Wheel 1:1',
'Pulley Wheel 1:1','Pulley Wheel 1:1',#11268,#11269,'Pulley Wheel 1:1');
#152=NEXT_ASSEMBLY_USAGE_OCCURRENCE('Radial Ball Bearing 1:1',
'Radial Ball Bearing 1:1','Radial Ball Bearing 1:1',#11268,#11270,
'Radial Ball Bearing 1:1');
#153=NEXT_ASSEMBLY_USAGE_OCCURRENCE('Radial Ball Bearing 2:1',
'Radial Ball Bearing 2:1','Radial Ball Bearing 2:1',#11268,#11271,
'Radial Ball Bearing 2:1');
#154=NEXT_ASSEMBLY_USAGE_OCCURRENCE('Pulley Wheel 2:1',
'Pulley Wheel 2:1','Pulley Wheel 2:1',#11268,#11272,'Pulley Wheel 2:1');
#155=NEXT_ASSEMBLY_USAGE_OCCURRENCE('Belt:1','Belt:1','Belt:1',#11268,#11273,
'Belt:1');
#156=NEXT_ASSEMBLY_USAGE_OCCURRENCE('Wheel Support:1','Wheel Support:1',
'Wheel Support:1',#11268,#11274,'Wheel Support:1');
#157=NEXT_ASSEMBLY_USAGE_OCCURRENCE('Radial Ball Bearing 3:1',
'Radial Ball Bearing 3:1','Radial Ball Bearing 3:1',#11268,#11275,
'Radial Ball Bearing 3:1');
#158=NEXT_ASSEMBLY_USAGE_OCCURRENCE('Mirror Front Support:1',
'Mirror Front Support:1','Mirror Front Support:1',#11268,#11276,
'Mirror Front Support:1');
#159=NEXT_ASSEMBLY_USAGE_OCCURRENCE('Radial Ball Bearing 4:1',
'Radial Ball Bearing 4:1','Radial Ball Bearing 4:1',#11268,#11277,
'Radial Ball Bearing 4:1');
#160=NEXT_ASSEMBLY_USAGE_OCCURRENCE('Broom Roller Assembly:1',
'Broom Roller Assembly:1','Broom Roller Assembly:1',#11268,#11278,
'Broom Roller Assembly:1');
#161=NEXT_ASSEMBLY_USAGE_OCCURRENCE('Body:1','Body:1','Body:1',#11268,#11286,
'Body:1');
#162=NEXT_ASSEMBLY_USAGE_OCCURRENCE('Ground Roller:1','Ground Roller:1',
'Ground Roller:1',#11268,#11287,'Ground Roller:1');
#163=NEXT_ASSEMBLY_USAGE_OCCURRENCE('Plate Assembly:1',
'Plate Assembly:1','Plate Assembly:1',#11268,#11288,'Plate Assembly:1');
#164=NEXT_ASSEMBLY_USAGE_OCCURRENCE('Push Handle Assembly:1',
'Push Handle Assembly:1','Push Handle Assembly:1',#11268,#11295,
'Push Handle Assembly:1');
#165=NEXT_ASSEMBLY_USAGE_OCCURRENCE('Front Support:1','Front Support:1',
'Front Support:1',#11268,#11301,'Front Support:1');
#166=NEXT_ASSEMBLY_USAGE_OCCURRENCE('Wheel Assembly:1',
'Wheel Assembly:1','Wheel Assembly:1',#11268,#11302,'Wheel Assembly:1');
#167=TOROIDAL_SURFACE('',#6462,0.0248999989285722,0.00110000131901909);
#168=TOROIDAL_SURFACE('',#6467,0.0248999989285722,0.00110000131901909);
#169=TOROIDAL_SURFACE('',#6475,0.0248999989285722,0.00110000131901911);
#170=TOROIDAL_SURFACE('',#6482,0.0248999989285722,0.00110000131901911);
#171=TOROIDAL_SURFACE('',#6486,0.01675,0.00555000054498457);
#172=TOROIDAL_SURFACE('',#6495,0.01675,0.00555000054498457);
#173=TOROIDAL_SURFACE('',#6504,0.00860000107142784,0.00110000131901912);
#174=TOROIDAL_SURFACE('',#6508,0.00860000107142784,0.00110000131901912);
#175=TOROIDAL_SURFACE('',#6516,0.00860000107142785,0.00110000131901912);
#176=TOROIDAL_SURFACE('',#6519,0.00860000107142785,0.00110000131901912);
#177=TOROIDAL_SURFACE('',#6521,0.0248999989285722,0.00110000131901909);
#178=TOROIDAL_SURFACE('',#6526,0.0248999989285722,0.00110000131901909);
#179=TOROIDAL_SURFACE('',#6534,0.0248999989285722,0.00110000131901911);
#180=TOROIDAL_SURFACE('',#6541,0.0248999989285722,0.00110000131901911);
#181=TOROIDAL_SURFACE('',#6545,0.01675,0.00555000054498457);
#182=TOROIDAL_SURFACE('',#6554,0.01675,0.00555000054498457);
#183=TOROIDAL_SURFACE('',#6563,0.00860000107142784,0.00110000131901912);
#184=TOROIDAL_SURFACE('',#6567,0.00860000107142784,0.00110000131901912);
#185=TOROIDAL_SURFACE('',#6575,0.00860000107142785,0.00110000131901912);
#186=TOROIDAL_SURFACE('',#6578,0.00860000107142785,0.00110000131901912);
#187=TOROIDAL_SURFACE('',#6680,0.0248999989285722,0.00110000131901909);
#188=TOROIDAL_SURFACE('',#6685,0.0248999989285722,0.00110000131901909);
#189=TOROIDAL_SURFACE('',#6693,0.0248999989285722,0.00110000131901911);
#190=TOROIDAL_SURFACE('',#6700,0.0248999989285722,0.00110000131901911);
#191=TOROIDAL_SURFACE('',#6704,0.01675,0.00555000054498457);
#192=TOROIDAL_SURFACE('',#6713,0.01675,0.00555000054498457);
#193=TOROIDAL_SURFACE('',#6722,0.00860000107142784,0.00110000131901912);
#194=TOROIDAL_SURFACE('',#6726,0.00860000107142784,0.00110000131901912);
#195=TOROIDAL_SURFACE('',#6734,0.00860000107142785,0.00110000131901912);
#196=TOROIDAL_SURFACE('',#6737,0.00860000107142785,0.00110000131901912);
#197=TOROIDAL_SURFACE('',#6769,0.0248999989285722,0.00110000131901909);
#198=TOROIDAL_SURFACE('',#6774,0.0248999989285722,0.00110000131901909);
#199=TOROIDAL_SURFACE('',#6782,0.0248999989285722,0.00110000131901911);
#200=TOROIDAL_SURFACE('',#6789,0.0248999989285722,0.00110000131901911);
#201=TOROIDAL_SURFACE('',#6793,0.01675,0.00555000054498457);
#202=TOROIDAL_SURFACE('',#6802,0.01675,0.00555000054498457);
#203=TOROIDAL_SURFACE('',#6811,0.00860000107142784,0.00110000131901912);
#204=TOROIDAL_SURFACE('',#6815,0.00860000107142784,0.00110000131901912);
#205=TOROIDAL_SURFACE('',#6823,0.00860000107142785,0.00110000131901912);
#206=TOROIDAL_SURFACE('',#6826,0.00860000107142785,0.00110000131901912);
#207=SHAPE_REPRESENTATION_RELATIONSHIP('SRR','None',#11230,#240);
#208=SHAPE_REPRESENTATION_RELATIONSHIP('SRR','None',#11231,#241);
#209=SHAPE_REPRESENTATION_RELATIONSHIP('SRR','None',#11232,#242);
#210=SHAPE_REPRESENTATION_RELATIONSHIP('SRR','None',#11233,#243);
#211=SHAPE_REPRESENTATION_RELATIONSHIP('SRR','None',#11234,#244);
#212=SHAPE_REPRESENTATION_RELATIONSHIP('SRR','None',#11235,#245);
#213=SHAPE_REPRESENTATION_RELATIONSHIP('SRR','None',#11236,#246);
#214=SHAPE_REPRESENTATION_RELATIONSHIP('SRR','None',#11237,#247);
#215=SHAPE_REPRESENTATION_RELATIONSHIP('SRR','None',#11238,#248);
#216=SHAPE_REPRESENTATION_RELATIONSHIP('SRR','None',#11240,#249);
#217=SHAPE_REPRESENTATION_RELATIONSHIP('SRR','None',#11241,#250);
#218=SHAPE_REPRESENTATION_RELATIONSHIP('SRR','None',#11242,#251);
#219=SHAPE_REPRESENTATION_RELATIONSHIP('SRR','None',#11243,#252);
#220=SHAPE_REPRESENTATION_RELATIONSHIP('SRR','None',#11244,#253);
#221=SHAPE_REPRESENTATION_RELATIONSHIP('SRR','None',#11245,#254);
#222=SHAPE_REPRESENTATION_RELATIONSHIP('SRR','None',#11246,#255);
#223=SHAPE_REPRESENTATION_RELATIONSHIP('SRR','None',#11247,#256);
#224=SHAPE_REPRESENTATION_RELATIONSHIP('SRR','None',#11248,#257);
#225=SHAPE_REPRESENTATION_RELATIONSHIP('SRR','None',#11250,#258);
#226=SHAPE_REPRESENTATION_RELATIONSHIP('SRR','None',#11251,#259);
#227=SHAPE_REPRESENTATION_RELATIONSHIP('SRR','None',#11252,#260);
#228=SHAPE_REPRESENTATION_RELATIONSHIP('SRR','None',#11253,#261);
#229=SHAPE_REPRESENTATION_RELATIONSHIP('SRR','None',#11254,#262);
#230=SHAPE_REPRESENTATION_RELATIONSHIP('SRR','None',#11255,#263);
#231=SHAPE_REPRESENTATION_RELATIONSHIP('SRR','None',#11257,#264);
#232=SHAPE_REPRESENTATION_RELATIONSHIP('SRR','None',#11258,#265);
#233=SHAPE_REPRESENTATION_RELATIONSHIP('SRR','None',#11259,#266);
#234=SHAPE_REPRESENTATION_RELATIONSHIP('SRR','None',#11260,#267);
#235=SHAPE_REPRESENTATION_RELATIONSHIP('SRR','None',#11261,#268);
#236=SHAPE_REPRESENTATION_RELATIONSHIP('SRR','None',#11262,#269);
#237=SHAPE_REPRESENTATION_RELATIONSHIP('SRR','None',#11264,#270);
#238=SHAPE_REPRESENTATION_RELATIONSHIP('SRR','None',#11265,#271);
#239=SHAPE_REPRESENTATION_RELATIONSHIP('SRR','None',#11266,#272);
#240=ADVANCED_BREP_SHAPE_REPRESENTATION('',(#306),#11075);
#241=ADVANCED_BREP_SHAPE_REPRESENTATION('',(#307),#11076);
#242=ADVANCED_BREP_SHAPE_REPRESENTATION('',(#308),#11077);
#243=ADVANCED_BREP_SHAPE_REPRESENTATION('',(#309),#11078);
#244=ADVANCED_BREP_SHAPE_REPRESENTATION('',(#310),#11079);
#245=ADVANCED_BREP_SHAPE_REPRESENTATION('',(#311),#11080);
#246=ADVANCED_BREP_SHAPE_REPRESENTATION('',(#312),#11081);
#247=ADVANCED_BREP_SHAPE_REPRESENTATION('',(#313),#11082);
#248=ADVANCED_BREP_SHAPE_REPRESENTATION('',(#314),#11083);
#249=ADVANCED_BREP_SHAPE_REPRESENTATION('',(#315),#11085);
#250=ADVANCED_BREP_SHAPE_REPRESENTATION('',(#316),#11086);
#251=ADVANCED_BREP_SHAPE_REPRESENTATION('',(#317),#11087);
#252=ADVANCED_BREP_SHAPE_REPRESENTATION('',(#318),#11088);
#253=ADVANCED_BREP_SHAPE_REPRESENTATION('',(#319),#11089);
#254=ADVANCED_BREP_SHAPE_REPRESENTATION('',(#320),#11090);
#255=ADVANCED_BREP_SHAPE_REPRESENTATION('',(#321),#11091);
#256=ADVANCED_BREP_SHAPE_REPRESENTATION('',(#322),#11092);
#257=ADVANCED_BREP_SHAPE_REPRESENTATION('',(#323),#11093);
#258=ADVANCED_BREP_SHAPE_REPRESENTATION('',(#324),#11095);
#259=ADVANCED_BREP_SHAPE_REPRESENTATION('',(#325),#11096);
#260=ADVANCED_BREP_SHAPE_REPRESENTATION('',(#326),#11097);
#261=ADVANCED_BREP_SHAPE_REPRESENTATION('',(#327),#11098);
#262=ADVANCED_BREP_SHAPE_REPRESENTATION('',(#328),#11099);
#263=ADVANCED_BREP_SHAPE_REPRESENTATION('',(#329),#11100);
#264=ADVANCED_BREP_SHAPE_REPRESENTATION('',(#330),#11102);
#265=ADVANCED_BREP_SHAPE_REPRESENTATION('',(#331),#11103);
#266=ADVANCED_BREP_SHAPE_REPRESENTATION('',(#332),#11104);
#267=ADVANCED_BREP_SHAPE_REPRESENTATION('',(#333),#11105);
#268=ADVANCED_BREP_SHAPE_REPRESENTATION('',(#334),#11106);
#269=ADVANCED_BREP_SHAPE_REPRESENTATION('',(#335),#11107);
#270=ADVANCED_BREP_SHAPE_REPRESENTATION('',(#336),#11109);
#271=ADVANCED_BREP_SHAPE_REPRESENTATION('',(#337),#11110);
#272=ADVANCED_BREP_SHAPE_REPRESENTATION('',(#338),#11111);
#273=STYLED_ITEM('',(#11424),#306);
#274=STYLED_ITEM('',(#11425),#307);
#275=STYLED_ITEM('',(#11425),#308);
#276=STYLED_ITEM('',(#11424),#309);
#277=STYLED_ITEM('',(#11426),#310);
#278=STYLED_ITEM('',(#11426),#311);
#279=STYLED_ITEM('',(#11425),#312);
#280=STYLED_ITEM('',(#11426),#313);
#281=STYLED_ITEM('',(#11425),#314);
#282=STYLED_ITEM('',(#11426),#315);
#283=STYLED_ITEM('',(#11426),#316);
#284=STYLED_ITEM('',(#11426),#317);
#285=STYLED_ITEM('',(#11426),#318);
#286=STYLED_ITEM('',(#11426),#319);
#287=STYLED_ITEM('',(#11426),#320);
#288=STYLED_ITEM('',(#11426),#321);
#289=STYLED_ITEM('',(#11426),#322);
#290=STYLED_ITEM('',(#11426),#323);
#291=STYLED_ITEM('',(#11426),#324);
#292=STYLED_ITEM('',(#11426),#325);
#293=STYLED_ITEM('',(#11426),#326);
#294=STYLED_ITEM('',(#11426),#327);
#295=STYLED_ITEM('',(#11426),#328);
#296=STYLED_ITEM('',(#11426),#329);
#297=STYLED_ITEM('',(#11426),#330);
#298=STYLED_ITEM('',(#11426),#331);
#299=STYLED_ITEM('',(#11426),#332);
#300=STYLED_ITEM('',(#11426),#333);
#301=STYLED_ITEM('',(#11426),#334);
#302=STYLED_ITEM('',(#11426),#335);
#303=STYLED_ITEM('',(#11426),#336);
#304=STYLED_ITEM('',(#11426),#337);
#305=STYLED_ITEM('',(#11426),#338);
#306=MANIFOLD_SOLID_BREP('Pulley Wheel 1',#6010);
#307=MANIFOLD_SOLID_BREP('Radial Ball Bearing 1',#6011);
#308=MANIFOLD_SOLID_BREP('Radial Ball Bearing 2',#6012);
#309=MANIFOLD_SOLID_BREP('Pulley Wheel 2',#6013);
#310=MANIFOLD_SOLID_BREP('Belt',#6014);
#311=MANIFOLD_SOLID_BREP('Wheel Support',#6015);
#312=MANIFOLD_SOLID_BREP('Radial Ball Bearing 3',#6016);
#313=MANIFOLD_SOLID_BREP('Mirror Front Support',#6017);
#314=MANIFOLD_SOLID_BREP('Radial Ball Bearing 4',#6018);
#315=MANIFOLD_SOLID_BREP('Broom Roller 1',#6019);
#316=MANIFOLD_SOLID_BREP('Broom Roller 2',#6020);
#317=MANIFOLD_SOLID_BREP('Broom Roller 3',#6021);
#318=MANIFOLD_SOLID_BREP('Broom Roller 4',#6022);
#319=MANIFOLD_SOLID_BREP('Broom Roller 5',#6023);
#320=MANIFOLD_SOLID_BREP('Broom Roller 6',#6024);
#321=MANIFOLD_SOLID_BREP('Broom Roller 7',#6025);
#322=MANIFOLD_SOLID_BREP('Body',#6026);
#323=MANIFOLD_SOLID_BREP('Ground Roller',#6027);
#324=MANIFOLD_SOLID_BREP('Plate 1',#6028);
#325=MANIFOLD_SOLID_BREP('Plate 2',#6029);
#326=MANIFOLD_SOLID_BREP('Plate 3',#6030);
#327=MANIFOLD_SOLID_BREP('Plate 4',#6031);
#328=MANIFOLD_SOLID_BREP('Plate 5',#6032);
#329=MANIFOLD_SOLID_BREP('Plate 6',#6033);
#330=MANIFOLD_SOLID_BREP('Push Handle 1',#6034);
#331=MANIFOLD_SOLID_BREP('Push Handle 2',#6035);
#332=MANIFOLD_SOLID_BREP('Push Handle 3',#6036);
#333=MANIFOLD_SOLID_BREP('Push Handle 4',#6037);
#334=MANIFOLD_SOLID_BREP('Push Handle 5',#6038);
#335=MANIFOLD_SOLID_BREP('Front Support',#6039);
#336=MANIFOLD_SOLID_BREP('Wheel 1',#6040);
#337=MANIFOLD_SOLID_BREP('Wheel 2',#6041);
#338=MANIFOLD_SOLID_BREP('Wheel 3',#6042);
#339=FACE_BOUND('',#1044,.T.);
#340=FACE_BOUND('',#1046,.T.);
#341=FACE_BOUND('',#1050,.T.);
#342=FACE_BOUND('',#1051,.T.);
#343=FACE_BOUND('',#1052,.T.);
#344=FACE_BOUND('',#1053,.T.);
#345=FACE_BOUND('',#1054,.T.);
#346=FACE_BOUND('',#1055,.T.);
#347=FACE_BOUND('',#1056,.T.);
#348=FACE_BOUND('',#1058,.T.);
#349=FACE_BOUND('',#1059,.T.);
#350=FACE_BOUND('',#1060,.T.);
#351=FACE_BOUND('',#1061,.T.);
#352=FACE_BOUND('',#1062,.T.);
#353=FACE_BOUND('',#1063,.T.);
#354=FACE_BOUND('',#1064,.T.);
#355=FACE_BOUND('',#1074,.T.);
#356=FACE_BOUND('',#1076,.T.);
#357=FACE_BOUND('',#1081,.T.);
#358=FACE_BOUND('',#1086,.T.);
#359=FACE_BOUND('',#1092,.T.);
#360=FACE_BOUND('',#1097,.T.);
#361=FACE_BOUND('',#1105,.T.);
#362=FACE_BOUND('',#1110,.T.);
#363=FACE_BOUND('',#1116,.T.);
#364=FACE_BOUND('',#1121,.T.);
#365=FACE_BOUND('',#1131,.T.);
#366=FACE_BOUND('',#1133,.T.);
#367=FACE_BOUND('',#1137,.T.);
#368=FACE_BOUND('',#1138,.T.);
#369=FACE_BOUND('',#1139,.T.);
#370=FACE_BOUND('',#1140,.T.);
#371=FACE_BOUND('',#1141,.T.);
#372=FACE_BOUND('',#1142,.T.);
#373=FACE_BOUND('',#1143,.T.);
#374=FACE_BOUND('',#1145,.T.);
#375=FACE_BOUND('',#1146,.T.);
#376=FACE_BOUND('',#1147,.T.);
#377=FACE_BOUND('',#1148,.T.);
#378=FACE_BOUND('',#1149,.T.);
#379=FACE_BOUND('',#1150,.T.);
#380=FACE_BOUND('',#1151,.T.);
#381=FACE_BOUND('',#1161,.T.);
#382=FACE_BOUND('',#1163,.T.);
#383=FACE_BOUND('',#1183,.T.);
#384=FACE_BOUND('',#1184,.T.);
#385=FACE_BOUND('',#1185,.T.);
#386=FACE_BOUND('',#1186,.T.);
#387=FACE_BOUND('',#1187,.T.);
#388=FACE_BOUND('',#1189,.T.);
#389=FACE_BOUND('',#1190,.T.);
#390=FACE_BOUND('',#1191,.T.);
#391=FACE_BOUND('',#1192,.T.);
#392=FACE_BOUND('',#1193,.T.);
#393=FACE_BOUND('',#1206,.T.);
#394=FACE_BOUND('',#1211,.T.);
#395=FACE_BOUND('',#1217,.T.);
#396=FACE_BOUND('',#1222,.T.);
#397=FACE_BOUND('',#1228,.T.);
#398=FACE_BOUND('',#1230,.T.);
#399=FACE_BOUND('',#1231,.T.);
#400=FACE_BOUND('',#1232,.T.);
#401=FACE_BOUND('',#1233,.T.);
#402=FACE_BOUND('',#1234,.T.);
#403=FACE_BOUND('',#1245,.T.);
#404=FACE_BOUND('',#1246,.T.);
#405=FACE_BOUND('',#1247,.T.);
#406=FACE_BOUND('',#1248,.T.);
#407=FACE_BOUND('',#1249,.T.);
#408=FACE_BOUND('',#1254,.T.);
#409=FACE_BOUND('',#1259,.T.);
#410=FACE_BOUND('',#1265,.T.);
#411=FACE_BOUND('',#1270,.T.);
#412=FACE_BOUND('',#1277,.T.);
#413=FACE_BOUND('',#1296,.T.);
#414=FACE_BOUND('',#1328,.T.);
#415=FACE_BOUND('',#1337,.T.);
#416=FACE_BOUND('',#1342,.T.);
#417=FACE_BOUND('',#1348,.T.);
#418=FACE_BOUND('',#1349,.T.);
#419=FACE_BOUND('',#1350,.T.);
#420=FACE_BOUND('',#1351,.T.);
#421=FACE_BOUND('',#1352,.T.);
#422=FACE_BOUND('',#1353,.T.);
#423=FACE_BOUND('',#1354,.T.);
#424=FACE_BOUND('',#1355,.T.);
#425=FACE_BOUND('',#1356,.T.);
#426=FACE_BOUND('',#1358,.T.);
#427=FACE_BOUND('',#1359,.T.);
#428=FACE_BOUND('',#1360,.T.);
#429=FACE_BOUND('',#1361,.T.);
#430=FACE_BOUND('',#1362,.T.);
#431=FACE_BOUND('',#1363,.T.);
#432=FACE_BOUND('',#1364,.T.);
#433=FACE_BOUND('',#1365,.T.);
#434=FACE_BOUND('',#1366,.T.);
#435=FACE_BOUND('',#1385,.T.);
#436=FACE_BOUND('',#1386,.T.);
#437=FACE_BOUND('',#1387,.T.);
#438=FACE_BOUND('',#1388,.T.);
#439=FACE_BOUND('',#1389,.T.);
#440=FACE_BOUND('',#1390,.T.);
#441=FACE_BOUND('',#1391,.T.);
#442=FACE_BOUND('',#1392,.T.);
#443=FACE_BOUND('',#1393,.T.);
#444=FACE_BOUND('',#1395,.T.);
#445=FACE_BOUND('',#1396,.T.);
#446=FACE_BOUND('',#1397,.T.);
#447=FACE_BOUND('',#1398,.T.);
#448=FACE_BOUND('',#1399,.T.);
#449=FACE_BOUND('',#1400,.T.);
#450=FACE_BOUND('',#1401,.T.);
#451=FACE_BOUND('',#1402,.T.);
#452=FACE_BOUND('',#1403,.T.);
#453=FACE_BOUND('',#1417,.T.);
#454=FACE_BOUND('',#1420,.T.);
#455=FACE_BOUND('',#1425,.T.);
#456=FACE_BOUND('',#1426,.T.);
#457=FACE_BOUND('',#1433,.T.);
#458=FACE_BOUND('',#1434,.T.);
#459=FACE_BOUND('',#1443,.T.);
#460=FACE_BOUND('',#1444,.T.);
#461=FACE_BOUND('',#1451,.T.);
#462=FACE_BOUND('',#1452,.T.);
#463=FACE_BOUND('',#1455,.T.);
#464=FACE_BOUND('',#1456,.T.);
#465=FACE_BOUND('',#1463,.T.);
#466=FACE_BOUND('',#1464,.T.);
#467=FACE_BOUND('',#1467,.T.);
#468=FACE_BOUND('',#1468,.T.);
#469=FACE_BOUND('',#1471,.T.);
#470=FACE_BOUND('',#1472,.T.);
#471=FACE_BOUND('',#1479,.T.);
#472=FACE_BOUND('',#1480,.T.);
#473=FACE_BOUND('',#1487,.T.);
#474=FACE_BOUND('',#1488,.T.);
#475=FACE_BOUND('',#1491,.T.);
#476=FACE_BOUND('',#1492,.T.);
#477=FACE_BOUND('',#1499,.T.);
#478=FACE_BOUND('',#1500,.T.);
#479=FACE_BOUND('',#1509,.T.);
#480=FACE_BOUND('',#1511,.T.);
#481=FACE_BOUND('',#1521,.T.);
#482=FACE_BOUND('',#1523,.T.);
#483=FACE_BOUND('',#1524,.T.);
#484=FACE_BOUND('',#1525,.T.);
#485=FACE_BOUND('',#1526,.T.);
#486=FACE_BOUND('',#1527,.T.);
#487=FACE_BOUND('',#1538,.T.);
#488=FACE_BOUND('',#1539,.T.);
#489=FACE_BOUND('',#1540,.T.);
#490=FACE_BOUND('',#1541,.T.);
#491=FACE_BOUND('',#1542,.T.);
#492=FACE_BOUND('',#1545,.T.);
#493=FACE_BOUND('',#1547,.T.);
#494=FACE_BOUND('',#1551,.T.);
#495=FACE_BOUND('',#1553,.T.);
#496=PLANE('',#6425);
#497=PLANE('',#6427);
#498=PLANE('',#6433);
#499=PLANE('',#6441);
#500=PLANE('',#6459);
#501=PLANE('',#6460);
#502=PLANE('',#6473);
#503=PLANE('',#6484);
#504=PLANE('',#6499);
#505=PLANE('',#6510);
#506=PLANE('',#6532);
#507=PLANE('',#6543);
#508=PLANE('',#6558);
#509=PLANE('',#6569);
#510=PLANE('',#6593);
#511=PLANE('',#6595);
#512=PLANE('',#6601);
#513=PLANE('',#6609);
#514=PLANE('',#6627);
#515=PLANE('',#6629);
#516=PLANE('',#6636);
#517=PLANE('',#6641);
#518=PLANE('',#6645);
#519=PLANE('',#6647);
#520=PLANE('',#6648);
#521=PLANE('',#6649);
#522=PLANE('',#6654);
#523=PLANE('',#6655);
#524=PLANE('',#6661);
#525=PLANE('',#6666);
#526=PLANE('',#6675);
#527=PLANE('',#6676);
#528=PLANE('',#6677);
#529=PLANE('',#6678);
#530=PLANE('',#6691);
#531=PLANE('',#6702);
#532=PLANE('',#6717);
#533=PLANE('',#6728);
#534=PLANE('',#6742);
#535=PLANE('',#6744);
#536=PLANE('',#6761);
#537=PLANE('',#6762);
#538=PLANE('',#6767);
#539=PLANE('',#6780);
#540=PLANE('',#6791);
#541=PLANE('',#6806);
#542=PLANE('',#6817);
#543=PLANE('',#6832);
#544=PLANE('',#6833);
#545=PLANE('',#6837);
#546=PLANE('',#6848);
#547=PLANE('',#6849);
#548=PLANE('',#6850);
#549=PLANE('',#6851);
#550=PLANE('',#6852);
#551=PLANE('',#6853);
#552=PLANE('',#6854);
#553=PLANE('',#6855);
#554=PLANE('',#6856);
#555=PLANE('',#6857);
#556=PLANE('',#6858);
#557=PLANE('',#6859);
#558=PLANE('',#6864);
#559=PLANE('',#6865);
#560=PLANE('',#6869);
#561=PLANE('',#6880);
#562=PLANE('',#6881);
#563=PLANE('',#6882);
#564=PLANE('',#6883);
#565=PLANE('',#6884);
#566=PLANE('',#6885);
#567=PLANE('',#6886);
#568=PLANE('',#6887);
#569=PLANE('',#6888);
#570=PLANE('',#6889);
#571=PLANE('',#6890);
#572=PLANE('',#6891);
#573=PLANE('',#6902);
#574=PLANE('',#6903);
#575=PLANE('',#6904);
#576=PLANE('',#6905);
#577=PLANE('',#6906);
#578=PLANE('',#6907);
#579=PLANE('',#6908);
#580=PLANE('',#6909);
#581=PLANE('',#6910);
#582=PLANE('',#6911);
#583=PLANE('',#6912);
#584=PLANE('',#6913);
#585=PLANE('',#6918);
#586=PLANE('',#6919);
#587=PLANE('',#6923);
#588=PLANE('',#6944);
#589=PLANE('',#6950);
#590=PLANE('',#6952);
#591=PLANE('',#6953);
#592=PLANE('',#6965);
#593=PLANE('',#6974);
#594=PLANE('',#6991);
#595=PLANE('',#6992);
#596=PLANE('',#6993);
#597=PLANE('',#6994);
#598=PLANE('',#6995);
#599=PLANE('',#6996);
#600=PLANE('',#6997);
#601=PLANE('',#6998);
#602=PLANE('',#6999);
#603=PLANE('',#7000);
#604=PLANE('',#7010);
#605=PLANE('',#7020);
#606=PLANE('',#7034);
#607=PLANE('',#7035);
#608=PLANE('',#7039);
#609=PLANE('',#7043);
#610=PLANE('',#7049);
#611=PLANE('',#7054);
#612=PLANE('',#7057);
#613=PLANE('',#7058);
#614=PLANE('',#7059);
#615=PLANE('',#7061);
#616=PLANE('',#7062);
#617=PLANE('',#7063);
#618=PLANE('',#7064);
#619=PLANE('',#7065);
#620=PLANE('',#7066);
#621=PLANE('',#7071);
#622=PLANE('',#7076);
#623=PLANE('',#7079);
#624=PLANE('',#7080);
#625=PLANE('',#7081);
#626=PLANE('',#7086);
#627=PLANE('',#7089);
#628=PLANE('',#7090);
#629=PLANE('',#7091);
#630=PLANE('',#7092);
#631=PLANE('',#7093);
#632=PLANE('',#7094);
#633=PLANE('',#7096);
#634=PLANE('',#7097);
#635=PLANE('',#7099);
#636=PLANE('',#7100);
#637=PLANE('',#7103);
#638=PLANE('',#7111);
#639=PLANE('',#7116);
#640=PLANE('',#7119);
#641=PLANE('',#7120);
#642=PLANE('',#7121);
#643=PLANE('',#7126);
#644=PLANE('',#7131);
#645=PLANE('',#7134);
#646=PLANE('',#7135);
#647=PLANE('',#7136);
#648=PLANE('',#7156);
#649=PLANE('',#7157);
#650=PLANE('',#7162);
#651=PLANE('',#7164);
#652=PLANE('',#7179);
#653=PLANE('',#7180);
#654=PLANE('',#7190);
#655=PLANE('',#7192);
#656=PLANE('',#7209);
#657=PLANE('',#7214);
#658=PLANE('',#7215);
#659=PLANE('',#7221);
#660=PLANE('',#7223);
#661=PLANE('',#7230);
#662=PLANE('',#7232);
#663=PLANE('',#7239);
#664=PLANE('',#7240);
#665=CONICAL_SURFACE('',#6416,1.,1.04719756558882);
#666=CONICAL_SURFACE('',#6418,1.,1.04719756558882);
#667=CONICAL_SURFACE('',#6584,1.,1.04719756558882);
#668=CONICAL_SURFACE('',#6586,1.,1.04719756558882);
#669=CONICAL_SURFACE('',#6637,1.,1.04719756558882);
#670=CONICAL_SURFACE('',#6639,1.,1.04719756558882);
#671=CONICAL_SURFACE('',#6650,1.,1.04719756558882);
#672=CONICAL_SURFACE('',#6652,1.,1.04719756558882);
#673=FACE_OUTER_BOUND('',#1037,.T.);
#674=FACE_OUTER_BOUND('',#1038,.T.);
#675=FACE_OUTER_BOUND('',#1039,.T.);
#676=FACE_OUTER_BOUND('',#1040,.T.);
#677=FACE_OUTER_BOUND('',#1041,.T.);
#678=FACE_OUTER_BOUND('',#1042,.T.);
#679=FACE_OUTER_BOUND('',#1043,.T.);
#680=FACE_OUTER_BOUND('',#1045,.T.);
#681=FACE_OUTER_BOUND('',#1047,.T.);
#682=FACE_OUTER_BOUND('',#1048,.T.);
#683=FACE_OUTER_BOUND('',#1049,.T.);
#684=FACE_OUTER_BOUND('',#1057,.T.);
#685=FACE_OUTER_BOUND('',#1065,.T.);
#686=FACE_OUTER_BOUND('',#1066,.T.);
#687=FACE_OUTER_BOUND('',#1067,.T.);
#688=FACE_OUTER_BOUND('',#1068,.T.);
#689=FACE_OUTER_BOUND('',#1069,.T.);
#690=FACE_OUTER_BOUND('',#1070,.T.);
#691=FACE_OUTER_BOUND('',#1071,.T.);
#692=FACE_OUTER_BOUND('',#1072,.T.);
#693=FACE_OUTER_BOUND('',#1073,.T.);
#694=FACE_OUTER_BOUND('',#1075,.T.);
#695=FACE_OUTER_BOUND('',#1077,.T.);
#696=FACE_OUTER_BOUND('',#1078,.T.);
#697=FACE_OUTER_BOUND('',#1079,.T.);
#698=FACE_OUTER_BOUND('',#1080,.T.);
#699=FACE_OUTER_BOUND('',#1082,.T.);
#700=FACE_OUTER_BOUND('',#1083,.T.);
#701=FACE_OUTER_BOUND('',#1084,.T.);
#702=FACE_OUTER_BOUND('',#1085,.T.);
#703=FACE_OUTER_BOUND('',#1087,.T.);
#704=FACE_OUTER_BOUND('',#1088,.T.);
#705=FACE_OUTER_BOUND('',#1089,.T.);
#706=FACE_OUTER_BOUND('',#1090,.T.);
#707=FACE_OUTER_BOUND('',#1091,.T.);
#708=FACE_OUTER_BOUND('',#1093,.T.);
#709=FACE_OUTER_BOUND('',#1094,.T.);
#710=FACE_OUTER_BOUND('',#1095,.T.);
#711=FACE_OUTER_BOUND('',#1096,.T.);
#712=FACE_OUTER_BOUND('',#1098,.T.);
#713=FACE_OUTER_BOUND('',#1099,.T.);
#714=FACE_OUTER_BOUND('',#1100,.T.);
#715=FACE_OUTER_BOUND('',#1101,.T.);
#716=FACE_OUTER_BOUND('',#1102,.T.);
#717=FACE_OUTER_BOUND('',#1103,.T.);
#718=FACE_OUTER_BOUND('',#1104,.T.);
#719=FACE_OUTER_BOUND('',#1106,.T.);
#720=FACE_OUTER_BOUND('',#1107,.T.);
#721=FACE_OUTER_BOUND('',#1108,.T.);
#722=FACE_OUTER_BOUND('',#1109,.T.);
#723=FACE_OUTER_BOUND('',#1111,.T.);
#724=FACE_OUTER_BOUND('',#1112,.T.);
#725=FACE_OUTER_BOUND('',#1113,.T.);
#726=FACE_OUTER_BOUND('',#1114,.T.);
#727=FACE_OUTER_BOUND('',#1115,.T.);
#728=FACE_OUTER_BOUND('',#1117,.T.);
#729=FACE_OUTER_BOUND('',#1118,.T.);
#730=FACE_OUTER_BOUND('',#1119,.T.);
#731=FACE_OUTER_BOUND('',#1120,.T.);
#732=FACE_OUTER_BOUND('',#1122,.T.);
#733=FACE_OUTER_BOUND('',#1123,.T.);
#734=FACE_OUTER_BOUND('',#1124,.T.);
#735=FACE_OUTER_BOUND('',#1125,.T.);
#736=FACE_OUTER_BOUND('',#1126,.T.);
#737=FACE_OUTER_BOUND('',#1127,.T.);
#738=FACE_OUTER_BOUND('',#1128,.T.);
#739=FACE_OUTER_BOUND('',#1129,.T.);
#740=FACE_OUTER_BOUND('',#1130,.T.);
#741=FACE_OUTER_BOUND('',#1132,.T.);
#742=FACE_OUTER_BOUND('',#1134,.T.);
#743=FACE_OUTER_BOUND('',#1135,.T.);
#744=FACE_OUTER_BOUND('',#1136,.T.);
#745=FACE_OUTER_BOUND('',#1144,.T.);
#746=FACE_OUTER_BOUND('',#1152,.T.);
#747=FACE_OUTER_BOUND('',#1153,.T.);
#748=FACE_OUTER_BOUND('',#1154,.T.);
#749=FACE_OUTER_BOUND('',#1155,.T.);
#750=FACE_OUTER_BOUND('',#1156,.T.);
#751=FACE_OUTER_BOUND('',#1157,.T.);
#752=FACE_OUTER_BOUND('',#1158,.T.);
#753=FACE_OUTER_BOUND('',#1159,.T.);
#754=FACE_OUTER_BOUND('',#1160,.T.);
#755=FACE_OUTER_BOUND('',#1162,.T.);
#756=FACE_OUTER_BOUND('',#1164,.T.);
#757=FACE_OUTER_BOUND('',#1165,.T.);
#758=FACE_OUTER_BOUND('',#1166,.T.);
#759=FACE_OUTER_BOUND('',#1167,.T.);
#760=FACE_OUTER_BOUND('',#1168,.T.);
#761=FACE_OUTER_BOUND('',#1169,.T.);
#762=FACE_OUTER_BOUND('',#1170,.T.);
#763=FACE_OUTER_BOUND('',#1171,.T.);
#764=FACE_OUTER_BOUND('',#1172,.T.);
#765=FACE_OUTER_BOUND('',#1173,.T.);
#766=FACE_OUTER_BOUND('',#1174,.T.);
#767=FACE_OUTER_BOUND('',#1175,.T.);
#768=FACE_OUTER_BOUND('',#1176,.T.);
#769=FACE_OUTER_BOUND('',#1177,.T.);
#770=FACE_OUTER_BOUND('',#1178,.T.);
#771=FACE_OUTER_BOUND('',#1179,.T.);
#772=FACE_OUTER_BOUND('',#1180,.T.);
#773=FACE_OUTER_BOUND('',#1181,.T.);
#774=FACE_OUTER_BOUND('',#1182,.T.);
#775=FACE_OUTER_BOUND('',#1188,.T.);
#776=FACE_OUTER_BOUND('',#1194,.T.);
#777=FACE_OUTER_BOUND('',#1195,.T.);
#778=FACE_OUTER_BOUND('',#1196,.T.);
#779=FACE_OUTER_BOUND('',#1197,.T.);
#780=FACE_OUTER_BOUND('',#1198,.T.);
#781=FACE_OUTER_BOUND('',#1199,.T.);
#782=FACE_OUTER_BOUND('',#1200,.T.);
#783=FACE_OUTER_BOUND('',#1201,.T.);
#784=FACE_OUTER_BOUND('',#1202,.T.);
#785=FACE_OUTER_BOUND('',#1203,.T.);
#786=FACE_OUTER_BOUND('',#1204,.T.);
#787=FACE_OUTER_BOUND('',#1205,.T.);
#788=FACE_OUTER_BOUND('',#1207,.T.);
#789=FACE_OUTER_BOUND('',#1208,.T.);
#790=FACE_OUTER_BOUND('',#1209,.T.);
#791=FACE_OUTER_BOUND('',#1210,.T.);
#792=FACE_OUTER_BOUND('',#1212,.T.);
#793=FACE_OUTER_BOUND('',#1213,.T.);
#794=FACE_OUTER_BOUND('',#1214,.T.);
#795=FACE_OUTER_BOUND('',#1215,.T.);
#796=FACE_OUTER_BOUND('',#1216,.T.);
#797=FACE_OUTER_BOUND('',#1218,.T.);
#798=FACE_OUTER_BOUND('',#1219,.T.);
#799=FACE_OUTER_BOUND('',#1220,.T.);
#800=FACE_OUTER_BOUND('',#1221,.T.);
#801=FACE_OUTER_BOUND('',#1223,.T.);
#802=FACE_OUTER_BOUND('',#1224,.T.);
#803=FACE_OUTER_BOUND('',#1225,.T.);
#804=FACE_OUTER_BOUND('',#1226,.T.);
#805=FACE_OUTER_BOUND('',#1227,.T.);
#806=FACE_OUTER_BOUND('',#1229,.T.);
#807=FACE_OUTER_BOUND('',#1235,.T.);
#808=FACE_OUTER_BOUND('',#1236,.T.);
#809=FACE_OUTER_BOUND('',#1237,.T.);
#810=FACE_OUTER_BOUND('',#1238,.T.);
#811=FACE_OUTER_BOUND('',#1239,.T.);
#812=FACE_OUTER_BOUND('',#1240,.T.);
#813=FACE_OUTER_BOUND('',#1241,.T.);
#814=FACE_OUTER_BOUND('',#1242,.T.);
#815=FACE_OUTER_BOUND('',#1243,.T.);
#816=FACE_OUTER_BOUND('',#1244,.T.);
#817=FACE_OUTER_BOUND('',#1250,.T.);
#818=FACE_OUTER_BOUND('',#1251,.T.);
#819=FACE_OUTER_BOUND('',#1252,.T.);
#820=FACE_OUTER_BOUND('',#1253,.T.);
#821=FACE_OUTER_BOUND('',#1255,.T.);
#822=FACE_OUTER_BOUND('',#1256,.T.);
#823=FACE_OUTER_BOUND('',#1257,.T.);
#824=FACE_OUTER_BOUND('',#1258,.T.);
#825=FACE_OUTER_BOUND('',#1260,.T.);
#826=FACE_OUTER_BOUND('',#1261,.T.);
#827=FACE_OUTER_BOUND('',#1262,.T.);
#828=FACE_OUTER_BOUND('',#1263,.T.);
#829=FACE_OUTER_BOUND('',#1264,.T.);
#830=FACE_OUTER_BOUND('',#1266,.T.);
#831=FACE_OUTER_BOUND('',#1267,.T.);
#832=FACE_OUTER_BOUND('',#1268,.T.);
#833=FACE_OUTER_BOUND('',#1269,.T.);
#834=FACE_OUTER_BOUND('',#1271,.T.);
#835=FACE_OUTER_BOUND('',#1272,.T.);
#836=FACE_OUTER_BOUND('',#1273,.T.);
#837=FACE_OUTER_BOUND('',#1274,.T.);
#838=FACE_OUTER_BOUND('',#1275,.T.);
#839=FACE_OUTER_BOUND('',#1276,.T.);
#840=FACE_OUTER_BOUND('',#1278,.T.);
#841=FACE_OUTER_BOUND('',#1279,.T.);
#842=FACE_OUTER_BOUND('',#1280,.T.);
#843=FACE_OUTER_BOUND('',#1281,.T.);
#844=FACE_OUTER_BOUND('',#1282,.T.);
#845=FACE_OUTER_BOUND('',#1283,.T.);
#846=FACE_OUTER_BOUND('',#1284,.T.);
#847=FACE_OUTER_BOUND('',#1285,.T.);
#848=FACE_OUTER_BOUND('',#1286,.T.);
#849=FACE_OUTER_BOUND('',#1287,.T.);
#850=FACE_OUTER_BOUND('',#1288,.T.);
#851=FACE_OUTER_BOUND('',#1289,.T.);
#852=FACE_OUTER_BOUND('',#1290,.T.);
#853=FACE_OUTER_BOUND('',#1291,.T.);
#854=FACE_OUTER_BOUND('',#1292,.T.);
#855=FACE_OUTER_BOUND('',#1293,.T.);
#856=FACE_OUTER_BOUND('',#1294,.T.);
#857=FACE_OUTER_BOUND('',#1295,.T.);
#858=FACE_OUTER_BOUND('',#1297,.T.);
#859=FACE_OUTER_BOUND('',#1298,.T.);
#860=FACE_OUTER_BOUND('',#1299,.T.);
#861=FACE_OUTER_BOUND('',#1300,.T.);
#862=FACE_OUTER_BOUND('',#1301,.T.);
#863=FACE_OUTER_BOUND('',#1302,.T.);
#864=FACE_OUTER_BOUND('',#1303,.T.);
#865=FACE_OUTER_BOUND('',#1304,.T.);
#866=FACE_OUTER_BOUND('',#1305,.T.);
#867=FACE_OUTER_BOUND('',#1306,.T.);
#868=FACE_OUTER_BOUND('',#1307,.T.);
#869=FACE_OUTER_BOUND('',#1308,.T.);
#870=FACE_OUTER_BOUND('',#1309,.T.);
#871=FACE_OUTER_BOUND('',#1310,.T.);
#872=FACE_OUTER_BOUND('',#1311,.T.);
#873=FACE_OUTER_BOUND('',#1312,.T.);
#874=FACE_OUTER_BOUND('',#1313,.T.);
#875=FACE_OUTER_BOUND('',#1314,.T.);
#876=FACE_OUTER_BOUND('',#1315,.T.);
#877=FACE_OUTER_BOUND('',#1316,.T.);
#878=FACE_OUTER_BOUND('',#1317,.T.);
#879=FACE_OUTER_BOUND('',#1318,.T.);
#880=FACE_OUTER_BOUND('',#1319,.T.);
#881=FACE_OUTER_BOUND('',#1320,.T.);
#882=FACE_OUTER_BOUND('',#1321,.T.);
#883=FACE_OUTER_BOUND('',#1322,.T.);
#884=FACE_OUTER_BOUND('',#1323,.T.);
#885=FACE_OUTER_BOUND('',#1324,.T.);
#886=FACE_OUTER_BOUND('',#1325,.T.);
#887=FACE_OUTER_BOUND('',#1326,.T.);
#888=FACE_OUTER_BOUND('',#1327,.T.);
#889=FACE_OUTER_BOUND('',#1329,.T.);
#890=FACE_OUTER_BOUND('',#1330,.T.);
#891=FACE_OUTER_BOUND('',#1331,.T.);
#892=FACE_OUTER_BOUND('',#1332,.T.);
#893=FACE_OUTER_BOUND('',#1333,.T.);
#894=FACE_OUTER_BOUND('',#1334,.T.);
#895=FACE_OUTER_BOUND('',#1335,.T.);
#896=FACE_OUTER_BOUND('',#1336,.T.);
#897=FACE_OUTER_BOUND('',#1338,.T.);
#898=FACE_OUTER_BOUND('',#1339,.T.);
#899=FACE_OUTER_BOUND('',#1340,.T.);
#900=FACE_OUTER_BOUND('',#1341,.T.);
#901=FACE_OUTER_BOUND('',#1343,.T.);
#902=FACE_OUTER_BOUND('',#1344,.T.);
#903=FACE_OUTER_BOUND('',#1345,.T.);
#904=FACE_OUTER_BOUND('',#1346,.T.);
#905=FACE_OUTER_BOUND('',#1347,.T.);
#906=FACE_OUTER_BOUND('',#1357,.T.);
#907=FACE_OUTER_BOUND('',#1367,.T.);
#908=FACE_OUTER_BOUND('',#1368,.T.);
#909=FACE_OUTER_BOUND('',#1369,.T.);
#910=FACE_OUTER_BOUND('',#1370,.T.);
#911=FACE_OUTER_BOUND('',#1371,.T.);
#912=FACE_OUTER_BOUND('',#1372,.T.);
#913=FACE_OUTER_BOUND('',#1373,.T.);
#914=FACE_OUTER_BOUND('',#1374,.T.);
#915=FACE_OUTER_BOUND('',#1375,.T.);
#916=FACE_OUTER_BOUND('',#1376,.T.);
#917=FACE_OUTER_BOUND('',#1377,.T.);
#918=FACE_OUTER_BOUND('',#1378,.T.);
#919=FACE_OUTER_BOUND('',#1379,.T.);
#920=FACE_OUTER_BOUND('',#1380,.T.);
#921=FACE_OUTER_BOUND('',#1381,.T.);
#922=FACE_OUTER_BOUND('',#1382,.T.);
#923=FACE_OUTER_BOUND('',#1383,.T.);
#924=FACE_OUTER_BOUND('',#1384,.T.);
#925=FACE_OUTER_BOUND('',#1394,.T.);
#926=FACE_OUTER_BOUND('',#1404,.T.);
#927=FACE_OUTER_BOUND('',#1405,.T.);
#928=FACE_OUTER_BOUND('',#1406,.T.);
#929=FACE_OUTER_BOUND('',#1407,.T.);
#930=FACE_OUTER_BOUND('',#1408,.T.);
#931=FACE_OUTER_BOUND('',#1409,.T.);
#932=FACE_OUTER_BOUND('',#1410,.T.);
#933=FACE_OUTER_BOUND('',#1411,.T.);
#934=FACE_OUTER_BOUND('',#1412,.T.);
#935=FACE_OUTER_BOUND('',#1413,.T.);
#936=FACE_OUTER_BOUND('',#1414,.T.);
#937=FACE_OUTER_BOUND('',#1415,.T.);
#938=FACE_OUTER_BOUND('',#1416,.T.);
#939=FACE_OUTER_BOUND('',#1418,.T.);
#940=FACE_OUTER_BOUND('',#1419,.T.);
#941=FACE_OUTER_BOUND('',#1421,.T.);
#942=FACE_OUTER_BOUND('',#1422,.T.);
#943=FACE_OUTER_BOUND('',#1423,.T.);
#944=FACE_OUTER_BOUND('',#1424,.T.);
#945=FACE_OUTER_BOUND('',#1427,.T.);
#946=FACE_OUTER_BOUND('',#1428,.T.);
#947=FACE_OUTER_BOUND('',#1429,.T.);
#948=FACE_OUTER_BOUND('',#1430,.T.);
#949=FACE_OUTER_BOUND('',#1431,.T.);
#950=FACE_OUTER_BOUND('',#1432,.T.);
#951=FACE_OUTER_BOUND('',#1435,.T.);
#952=FACE_OUTER_BOUND('',#1436,.T.);
#953=FACE_OUTER_BOUND('',#1437,.T.);
#954=FACE_OUTER_BOUND('',#1438,.T.);
#955=FACE_OUTER_BOUND('',#1439,.T.);
#956=FACE_OUTER_BOUND('',#1440,.T.);
#957=FACE_OUTER_BOUND('',#1441,.T.);
#958=FACE_OUTER_BOUND('',#1442,.T.);
#959=FACE_OUTER_BOUND('',#1445,.T.);
#960=FACE_OUTER_BOUND('',#1446,.T.);
#961=FACE_OUTER_BOUND('',#1447,.T.);
#962=FACE_OUTER_BOUND('',#1448,.T.);
#963=FACE_OUTER_BOUND('',#1449,.T.);
#964=FACE_OUTER_BOUND('',#1450,.T.);
#965=FACE_OUTER_BOUND('',#1453,.T.);
#966=FACE_OUTER_BOUND('',#1454,.T.);
#967=FACE_OUTER_BOUND('',#1457,.T.);
#968=FACE_OUTER_BOUND('',#1458,.T.);
#969=FACE_OUTER_BOUND('',#1459,.T.);
#970=FACE_OUTER_BOUND('',#1460,.T.);
#971=FACE_OUTER_BOUND('',#1461,.T.);
#972=FACE_OUTER_BOUND('',#1462,.T.);
#973=FACE_OUTER_BOUND('',#1465,.T.);
#974=FACE_OUTER_BOUND('',#1466,.T.);
#975=FACE_OUTER_BOUND('',#1469,.T.);
#976=FACE_OUTER_BOUND('',#1470,.T.);
#977=FACE_OUTER_BOUND('',#1473,.T.);
#978=FACE_OUTER_BOUND('',#1474,.T.);
#979=FACE_OUTER_BOUND('',#1475,.T.);
#980=FACE_OUTER_BOUND('',#1476,.T.);
#981=FACE_OUTER_BOUND('',#1477,.T.);
#982=FACE_OUTER_BOUND('',#1478,.T.);
#983=FACE_OUTER_BOUND('',#1481,.T.);
#984=FACE_OUTER_BOUND('',#1482,.T.);
#985=FACE_OUTER_BOUND('',#1483,.T.);
#986=FACE_OUTER_BOUND('',#1484,.T.);
#987=FACE_OUTER_BOUND('',#1485,.T.);
#988=FACE_OUTER_BOUND('',#1486,.T.);
#989=FACE_OUTER_BOUND('',#1489,.T.);
#990=FACE_OUTER_BOUND('',#1490,.T.);
#991=FACE_OUTER_BOUND('',#1493,.T.);
#992=FACE_OUTER_BOUND('',#1494,.T.);
#993=FACE_OUTER_BOUND('',#1495,.T.);
#994=FACE_OUTER_BOUND('',#1496,.T.);
#995=FACE_OUTER_BOUND('',#1497,.T.);
#996=FACE_OUTER_BOUND('',#1498,.T.);
#997=FACE_OUTER_BOUND('',#1501,.T.);
#998=FACE_OUTER_BOUND('',#1502,.T.);
#999=FACE_OUTER_BOUND('',#1503,.T.);
#1000=FACE_OUTER_BOUND('',#1504,.T.);
#1001=FACE_OUTER_BOUND('',#1505,.T.);
#1002=FACE_OUTER_BOUND('',#1506,.T.);
#1003=FACE_OUTER_BOUND('',#1507,.T.);
#1004=FACE_OUTER_BOUND('',#1508,.T.);
#1005=FACE_OUTER_BOUND('',#1510,.T.);
#1006=FACE_OUTER_BOUND('',#1512,.T.);
#1007=FACE_OUTER_BOUND('',#1513,.T.);
#1008=FACE_OUTER_BOUND('',#1514,.T.);
#1009=FACE_OUTER_BOUND('',#1515,.T.);
#1010=FACE_OUTER_BOUND('',#1516,.T.);
#1011=FACE_OUTER_BOUND('',#1517,.T.);
#1012=FACE_OUTER_BOUND('',#1518,.T.);
#1013=FACE_OUTER_BOUND('',#1519,.T.);
#1014=FACE_OUTER_BOUND('',#1520,.T.);
#1015=FACE_OUTER_BOUND('',#1522,.T.);
#1016=FACE_OUTER_BOUND('',#1528,.T.);
#1017=FACE_OUTER_BOUND('',#1529,.T.);
#1018=FACE_OUTER_BOUND('',#1530,.T.);
#1019=FACE_OUTER_BOUND('',#1531,.T.);
#1020=FACE_OUTER_BOUND('',#1532,.T.);
#1021=FACE_OUTER_BOUND('',#1533,.T.);
#1022=FACE_OUTER_BOUND('',#1534,.T.);
#1023=FACE_OUTER_BOUND('',#1535,.T.);
#1024=FACE_OUTER_BOUND('',#1536,.T.);
#1025=FACE_OUTER_BOUND('',#1537,.T.);
#1026=FACE_OUTER_BOUND('',#1543,.T.);
#1027=FACE_OUTER_BOUND('',#1544,.T.);
#1028=FACE_OUTER_BOUND('',#1546,.T.);
#1029=FACE_OUTER_BOUND('',#1548,.T.);
#1030=FACE_OUTER_BOUND('',#1549,.T.);
#1031=FACE_OUTER_BOUND('',#1550,.T.);
#1032=FACE_OUTER_BOUND('',#1552,.T.);
#1033=FACE_OUTER_BOUND('',#1554,.T.);
#1034=FACE_OUTER_BOUND('',#1555,.T.);
#1035=FACE_OUTER_BOUND('',#1556,.T.);
#1036=FACE_OUTER_BOUND('',#1557,.T.);
#1037=EDGE_LOOP('',(#3953,#3954,#3955,#3956));
#1038=EDGE_LOOP('',(#3957,#3958,#3959,#3960,#3961));
#1039=EDGE_LOOP('',(#3962,#3963,#3964,#3965,#3966));
#1040=EDGE_LOOP('',(#3967,#3968,#3969,#3970,#3971));
#1041=EDGE_LOOP('',(#3972,#3973,#3974,#3975));
#1042=EDGE_LOOP('',(#3976,#3977,#3978,#3979,#3980));
#1043=EDGE_LOOP('',(#3981));
#1044=EDGE_LOOP('',(#3982));
#1045=EDGE_LOOP('',(#3983));
#1046=EDGE_LOOP('',(#3984));
#1047=EDGE_LOOP('',(#3985,#3986,#3987,#3988));
#1048=EDGE_LOOP('',(#3989,#3990,#3991,#3992));
#1049=EDGE_LOOP('',(#3993));
#1050=EDGE_LOOP('',(#3994));
#1051=EDGE_LOOP('',(#3995));
#1052=EDGE_LOOP('',(#3996));
#1053=EDGE_LOOP('',(#3997));
#1054=EDGE_LOOP('',(#3998));
#1055=EDGE_LOOP('',(#3999));
#1056=EDGE_LOOP('',(#4000));
#1057=EDGE_LOOP('',(#4001));
#1058=EDGE_LOOP('',(#4002));
#1059=EDGE_LOOP('',(#4003));
#1060=EDGE_LOOP('',(#4004));
#1061=EDGE_LOOP('',(#4005));
#1062=EDGE_LOOP('',(#4006));
#1063=EDGE_LOOP('',(#4007));
#1064=EDGE_LOOP('',(#4008));
#1065=EDGE_LOOP('',(#4009,#4010,#4011,#4012));
#1066=EDGE_LOOP('',(#4013,#4014,#4015,#4016));
#1067=EDGE_LOOP('',(#4017,#4018,#4019,#4020));
#1068=EDGE_LOOP('',(#4021,#4022,#4023,#4024));
#1069=EDGE_LOOP('',(#4025,#4026,#4027,#4028));
#1070=EDGE_LOOP('',(#4029,#4030,#4031,#4032));
#1071=EDGE_LOOP('',(#4033,#4034,#4035,#4036));
#1072=EDGE_LOOP('',(#4037,#4038,#4039,#4040));
#1073=EDGE_LOOP('',(#4041));
#1074=EDGE_LOOP('',(#4042));
#1075=EDGE_LOOP('',(#4043));
#1076=EDGE_LOOP('',(#4044));
#1077=EDGE_LOOP('',(#4045,#4046,#4047,#4048));
#1078=EDGE_LOOP('',(#4049,#4050,#4051,#4052));
#1079=EDGE_LOOP('',(#4053,#4054,#4055,#4056,#4057,#4058));
#1080=EDGE_LOOP('',(#4059,#4060));
#1081=EDGE_LOOP('',(#4061));
#1082=EDGE_LOOP('',(#4062,#4063,#4064,#4065));
#1083=EDGE_LOOP('',(#4066,#4067,#4068,#4069,#4070));
#1084=EDGE_LOOP('',(#4071,#4072,#4073,#4074));
#1085=EDGE_LOOP('',(#4075,#4076));
#1086=EDGE_LOOP('',(#4077));
#1087=EDGE_LOOP('',(#4078,#4079,#4080,#4081,#4082,#4083));
#1088=EDGE_LOOP('',(#4084,#4085,#4086,#4087,#4088));
#1089=EDGE_LOOP('',(#4089,#4090,#4091,#4092,#4093));
#1090=EDGE_LOOP('',(#4094,#4095,#4096,#4097,#4098,#4099));
#1091=EDGE_LOOP('',(#4100));
#1092=EDGE_LOOP('',(#4101,#4102));
#1093=EDGE_LOOP('',(#4103,#4104,#4105,#4106,#4107));
#1094=EDGE_LOOP('',(#4108,#4109,#4110,#4111));
#1095=EDGE_LOOP('',(#4112,#4113,#4114,#4115));
#1096=EDGE_LOOP('',(#4116));
#1097=EDGE_LOOP('',(#4117,#4118));
#1098=EDGE_LOOP('',(#4119,#4120,#4121,#4122,#4123,#4124));
#1099=EDGE_LOOP('',(#4125,#4126,#4127,#4128));
#1100=EDGE_LOOP('',(#4129,#4130,#4131,#4132));
#1101=EDGE_LOOP('',(#4133,#4134,#4135,#4136));
#1102=EDGE_LOOP('',(#4137,#4138,#4139,#4140));
#1103=EDGE_LOOP('',(#4141,#4142,#4143,#4144,#4145,#4146));
#1104=EDGE_LOOP('',(#4147,#4148));
#1105=EDGE_LOOP('',(#4149));
#1106=EDGE_LOOP('',(#4150,#4151,#4152,#4153));
#1107=EDGE_LOOP('',(#4154,#4155,#4156,#4157,#4158));
#1108=EDGE_LOOP('',(#4159,#4160,#4161,#4162));
#1109=EDGE_LOOP('',(#4163,#4164));
#1110=EDGE_LOOP('',(#4165));
#1111=EDGE_LOOP('',(#4166,#4167,#4168,#4169,#4170,#4171));
#1112=EDGE_LOOP('',(#4172,#4173,#4174,#4175,#4176));
#1113=EDGE_LOOP('',(#4177,#4178,#4179,#4180,#4181));
#1114=EDGE_LOOP('',(#4182,#4183,#4184,#4185,#4186,#4187));
#1115=EDGE_LOOP('',(#4188));
#1116=EDGE_LOOP('',(#4189,#4190));
#1117=EDGE_LOOP('',(#4191,#4192,#4193,#4194,#4195));
#1118=EDGE_LOOP('',(#4196,#4197,#4198,#4199));
#1119=EDGE_LOOP('',(#4200,#4201,#4202,#4203));
#1120=EDGE_LOOP('',(#4204));
#1121=EDGE_LOOP('',(#4205,#4206));
#1122=EDGE_LOOP('',(#4207,#4208,#4209,#4210,#4211,#4212));
#1123=EDGE_LOOP('',(#4213,#4214,#4215,#4216));
#1124=EDGE_LOOP('',(#4217,#4218,#4219,#4220));
#1125=EDGE_LOOP('',(#4221,#4222,#4223,#4224,#4225));
#1126=EDGE_LOOP('',(#4226,#4227,#4228,#4229,#4230));
#1127=EDGE_LOOP('',(#4231,#4232,#4233,#4234,#4235));
#1128=EDGE_LOOP('',(#4236,#4237,#4238,#4239));
#1129=EDGE_LOOP('',(#4240,#4241,#4242,#4243,#4244));
#1130=EDGE_LOOP('',(#4245));
#1131=EDGE_LOOP('',(#4246));
#1132=EDGE_LOOP('',(#4247));
#1133=EDGE_LOOP('',(#4248));
#1134=EDGE_LOOP('',(#4249,#4250,#4251,#4252));
#1135=EDGE_LOOP('',(#4253,#4254,#4255,#4256));
#1136=EDGE_LOOP('',(#4257));
#1137=EDGE_LOOP('',(#4258));
#1138=EDGE_LOOP('',(#4259));
#1139=EDGE_LOOP('',(#4260));
#1140=EDGE_LOOP('',(#4261));
#1141=EDGE_LOOP('',(#4262));
#1142=EDGE_LOOP('',(#4263));
#1143=EDGE_LOOP('',(#4264));
#1144=EDGE_LOOP('',(#4265));
#1145=EDGE_LOOP('',(#4266));
#1146=EDGE_LOOP('',(#4267));
#1147=EDGE_LOOP('',(#4268));
#1148=EDGE_LOOP('',(#4269));
#1149=EDGE_LOOP('',(#4270));
#1150=EDGE_LOOP('',(#4271));
#1151=EDGE_LOOP('',(#4272));
#1152=EDGE_LOOP('',(#4273,#4274,#4275,#4276));
#1153=EDGE_LOOP('',(#4277,#4278,#4279,#4280));
#1154=EDGE_LOOP('',(#4281,#4282,#4283,#4284));
#1155=EDGE_LOOP('',(#4285,#4286,#4287,#4288));
#1156=EDGE_LOOP('',(#4289,#4290,#4291,#4292));
#1157=EDGE_LOOP('',(#4293,#4294,#4295,#4296));
#1158=EDGE_LOOP('',(#4297,#4298,#4299,#4300));
#1159=EDGE_LOOP('',(#4301,#4302,#4303,#4304));
#1160=EDGE_LOOP('',(#4305));
#1161=EDGE_LOOP('',(#4306));
#1162=EDGE_LOOP('',(#4307));
#1163=EDGE_LOOP('',(#4308));
#1164=EDGE_LOOP('',(#4309,#4310,#4311,#4312));
#1165=EDGE_LOOP('',(#4313,#4314,#4315,#4316));
#1166=EDGE_LOOP('',(#4317,#4318,#4319,#4320));
#1167=EDGE_LOOP('',(#4321,#4322,#4323,#4324));
#1168=EDGE_LOOP('',(#4325,#4326,#4327,#4328));
#1169=EDGE_LOOP('',(#4329,#4330,#4331,#4332));
#1170=EDGE_LOOP('',(#4333,#4334,#4335,#4336));
#1171=EDGE_LOOP('',(#4337,#4338,#4339,#4340));
#1172=EDGE_LOOP('',(#4341,#4342,#4343,#4344));
#1173=EDGE_LOOP('',(#4345,#4346,#4347,#4348));
#1174=EDGE_LOOP('',(#4349,#4350,#4351,#4352));
#1175=EDGE_LOOP('',(#4353,#4354,#4355,#4356));
#1176=EDGE_LOOP('',(#4357,#4358,#4359,#4360));
#1177=EDGE_LOOP('',(#4361,#4362,#4363,#4364));
#1178=EDGE_LOOP('',(#4365,#4366,#4367,#4368));
#1179=EDGE_LOOP('',(#4369,#4370,#4371,#4372));
#1180=EDGE_LOOP('',(#4373,#4374,#4375,#4376));
#1181=EDGE_LOOP('',(#4377,#4378,#4379,#4380));
#1182=EDGE_LOOP('',(#4381,#4382,#4383,#4384));
#1183=EDGE_LOOP('',(#4385));
#1184=EDGE_LOOP('',(#4386));
#1185=EDGE_LOOP('',(#4387));
#1186=EDGE_LOOP('',(#4388));
#1187=EDGE_LOOP('',(#4389));
#1188=EDGE_LOOP('',(#4390,#4391,#4392,#4393));
#1189=EDGE_LOOP('',(#4394));
#1190=EDGE_LOOP('',(#4395));
#1191=EDGE_LOOP('',(#4396));
#1192=EDGE_LOOP('',(#4397));
#1193=EDGE_LOOP('',(#4398));
#1194=EDGE_LOOP('',(#4399,#4400,#4401,#4402));
#1195=EDGE_LOOP('',(#4403,#4404,#4405,#4406));
#1196=EDGE_LOOP('',(#4407,#4408,#4409,#4410));
#1197=EDGE_LOOP('',(#4411,#4412,#4413,#4414));
#1198=EDGE_LOOP('',(#4415,#4416,#4417,#4418));
#1199=EDGE_LOOP('',(#4419,#4420,#4421,#4422));
#1200=EDGE_LOOP('',(#4423,#4424,#4425,#4426));
#1201=EDGE_LOOP('',(#4427,#4428,#4429,#4430));
#1202=EDGE_LOOP('',(#4431,#4432,#4433,#4434));
#1203=EDGE_LOOP('',(#4435,#4436,#4437,#4438));
#1204=EDGE_LOOP('',(#4439,#4440,#4441,#4442,#4443,#4444));
#1205=EDGE_LOOP('',(#4445,#4446));
#1206=EDGE_LOOP('',(#4447));
#1207=EDGE_LOOP('',(#4448,#4449,#4450,#4451));
#1208=EDGE_LOOP('',(#4452,#4453,#4454,#4455,#4456));
#1209=EDGE_LOOP('',(#4457,#4458,#4459,#4460));
#1210=EDGE_LOOP('',(#4461,#4462));
#1211=EDGE_LOOP('',(#4463));
#1212=EDGE_LOOP('',(#4464,#4465,#4466,#4467,#4468,#4469));
#1213=EDGE_LOOP('',(#4470,#4471,#4472,#4473,#4474));
#1214=EDGE_LOOP('',(#4475,#4476,#4477,#4478,#4479));
#1215=EDGE_LOOP('',(#4480,#4481,#4482,#4483,#4484,#4485));
#1216=EDGE_LOOP('',(#4486));
#1217=EDGE_LOOP('',(#4487,#4488));
#1218=EDGE_LOOP('',(#4489,#4490,#4491,#4492,#4493));
#1219=EDGE_LOOP('',(#4494,#4495,#4496,#4497));
#1220=EDGE_LOOP('',(#4498,#4499,#4500,#4501));
#1221=EDGE_LOOP('',(#4502));
#1222=EDGE_LOOP('',(#4503,#4504));
#1223=EDGE_LOOP('',(#4505,#4506,#4507,#4508,#4509,#4510));
#1224=EDGE_LOOP('',(#4511,#4512,#4513,#4514));
#1225=EDGE_LOOP('',(#4515,#4516,#4517,#4518));
#1226=EDGE_LOOP('',(#4519,#4520,#4521,#4522));
#1227=EDGE_LOOP('',(#4523));
#1228=EDGE_LOOP('',(#4524));
#1229=EDGE_LOOP('',(#4525,#4526,#4527,#4528));
#1230=EDGE_LOOP('',(#4529));
#1231=EDGE_LOOP('',(#4530));
#1232=EDGE_LOOP('',(#4531));
#1233=EDGE_LOOP('',(#4532));
#1234=EDGE_LOOP('',(#4533));
#1235=EDGE_LOOP('',(#4534,#4535,#4536,#4537));
#1236=EDGE_LOOP('',(#4538,#4539,#4540,#4541));
#1237=EDGE_LOOP('',(#4542,#4543,#4544,#4545));
#1238=EDGE_LOOP('',(#4546,#4547,#4548,#4549));
#1239=EDGE_LOOP('',(#4550,#4551,#4552,#4553));
#1240=EDGE_LOOP('',(#4554,#4555,#4556,#4557));
#1241=EDGE_LOOP('',(#4558,#4559,#4560,#4561));
#1242=EDGE_LOOP('',(#4562,#4563,#4564,#4565));
#1243=EDGE_LOOP('',(#4566,#4567,#4568,#4569));
#1244=EDGE_LOOP('',(#4570,#4571,#4572,#4573));
#1245=EDGE_LOOP('',(#4574));
#1246=EDGE_LOOP('',(#4575));
#1247=EDGE_LOOP('',(#4576));
#1248=EDGE_LOOP('',(#4577));
#1249=EDGE_LOOP('',(#4578));
#1250=EDGE_LOOP('',(#4579,#4580,#4581,#4582));
#1251=EDGE_LOOP('',(#4583,#4584,#4585,#4586));
#1252=EDGE_LOOP('',(#4587,#4588,#4589,#4590,#4591,#4592));
#1253=EDGE_LOOP('',(#4593,#4594));
#1254=EDGE_LOOP('',(#4595));
#1255=EDGE_LOOP('',(#4596,#4597,#4598,#4599));
#1256=EDGE_LOOP('',(#4600,#4601,#4602,#4603,#4604));
#1257=EDGE_LOOP('',(#4605,#4606,#4607,#4608));
#1258=EDGE_LOOP('',(#4609,#4610));
#1259=EDGE_LOOP('',(#4611));
#1260=EDGE_LOOP('',(#4612,#4613,#4614,#4615,#4616,#4617));
#1261=EDGE_LOOP('',(#4618,#4619,#4620,#4621,#4622));
#1262=EDGE_LOOP('',(#4623,#4624,#4625,#4626,#4627));
#1263=EDGE_LOOP('',(#4628,#4629,#4630,#4631,#4632,#4633));
#1264=EDGE_LOOP('',(#4634));
#1265=EDGE_LOOP('',(#4635,#4636));
#1266=EDGE_LOOP('',(#4637,#4638,#4639,#4640,#4641));
#1267=EDGE_LOOP('',(#4642,#4643,#4644,#4645));
#1268=EDGE_LOOP('',(#4646,#4647,#4648,#4649));
#1269=EDGE_LOOP('',(#4650));
#1270=EDGE_LOOP('',(#4651,#4652));
#1271=EDGE_LOOP('',(#4653,#4654,#4655,#4656,#4657,#4658));
#1272=EDGE_LOOP('',(#4659,#4660,#4661,#4662));
#1273=EDGE_LOOP('',(#4663,#4664,#4665,#4666));
#1274=EDGE_LOOP('',(#4667,#4668,#4669,#4670));
#1275=EDGE_LOOP('',(#4671));
#1276=EDGE_LOOP('',(#4672));
#1277=EDGE_LOOP('',(#4673));
#1278=EDGE_LOOP('',(#4674,#4675,#4676,#4677));
#1279=EDGE_LOOP('',(#4678));
#1280=EDGE_LOOP('',(#4679,#4680,#4681,#4682,#4683,#4684,#4685,#4686,#4687,
#4688));
#1281=EDGE_LOOP('',(#4689));
#1282=EDGE_LOOP('',(#4690,#4691,#4692));
#1283=EDGE_LOOP('',(#4693,#4694,#4695));
#1284=EDGE_LOOP('',(#4696,#4697,#4698));
#1285=EDGE_LOOP('',(#4699,#4700));
#1286=EDGE_LOOP('',(#4701,#4702,#4703));
#1287=EDGE_LOOP('',(#4704,#4705,#4706));
#1288=EDGE_LOOP('',(#4707,#4708,#4709,#4710,#4711,#4712));
#1289=EDGE_LOOP('',(#4713,#4714,#4715,#4716,#4717));
#1290=EDGE_LOOP('',(#4718,#4719,#4720,#4721,#4722,#4723));
#1291=EDGE_LOOP('',(#4724,#4725,#4726,#4727,#4728));
#1292=EDGE_LOOP('',(#4729,#4730,#4731,#4732));
#1293=EDGE_LOOP('',(#4733,#4734,#4735,#4736));
#1294=EDGE_LOOP('',(#4737));
#1295=EDGE_LOOP('',(#4738));
#1296=EDGE_LOOP('',(#4739));
#1297=EDGE_LOOP('',(#4740,#4741,#4742,#4743));
#1298=EDGE_LOOP('',(#4744));
#1299=EDGE_LOOP('',(#4745,#4746,#4747,#4748,#4749,#4750,#4751,#4752,#4753,
#4754));
#1300=EDGE_LOOP('',(#4755));
#1301=EDGE_LOOP('',(#4756,#4757,#4758));
#1302=EDGE_LOOP('',(#4759,#4760,#4761));
#1303=EDGE_LOOP('',(#4762,#4763,#4764));
#1304=EDGE_LOOP('',(#4765,#4766));
#1305=EDGE_LOOP('',(#4767,#4768,#4769));
#1306=EDGE_LOOP('',(#4770,#4771,#4772));
#1307=EDGE_LOOP('',(#4773,#4774,#4775,#4776,#4777,#4778));
#1308=EDGE_LOOP('',(#4779,#4780,#4781,#4782,#4783));
#1309=EDGE_LOOP('',(#4784,#4785,#4786,#4787,#4788,#4789));
#1310=EDGE_LOOP('',(#4790,#4791,#4792,#4793,#4794));
#1311=EDGE_LOOP('',(#4795,#4796,#4797,#4798));
#1312=EDGE_LOOP('',(#4799,#4800,#4801,#4802,#4803,#4804,#4805,#4806,#4807,
#4808));
#1313=EDGE_LOOP('',(#4809));
#1314=EDGE_LOOP('',(#4810,#4811,#4812));
#1315=EDGE_LOOP('',(#4813,#4814,#4815));
#1316=EDGE_LOOP('',(#4816,#4817,#4818));
#1317=EDGE_LOOP('',(#4819,#4820));
#1318=EDGE_LOOP('',(#4821,#4822,#4823));
#1319=EDGE_LOOP('',(#4824,#4825,#4826));
#1320=EDGE_LOOP('',(#4827,#4828,#4829,#4830,#4831,#4832));
#1321=EDGE_LOOP('',(#4833,#4834,#4835,#4836,#4837));
#1322=EDGE_LOOP('',(#4838,#4839,#4840,#4841,#4842,#4843));
#1323=EDGE_LOOP('',(#4844,#4845,#4846,#4847,#4848));
#1324=EDGE_LOOP('',(#4849,#4850,#4851,#4852));
#1325=EDGE_LOOP('',(#4853,#4854,#4855,#4856));
#1326=EDGE_LOOP('',(#4857));
#1327=EDGE_LOOP('',(#4858));
#1328=EDGE_LOOP('',(#4859));
#1329=EDGE_LOOP('',(#4860,#4861,#4862,#4863));
#1330=EDGE_LOOP('',(#4864));
#1331=EDGE_LOOP('',(#4865,#4866,#4867,#4868,#4869,#4870));
#1332=EDGE_LOOP('',(#4871,#4872,#4873,#4874,#4875));
#1333=EDGE_LOOP('',(#4876,#4877,#4878,#4879,#4880));
#1334=EDGE_LOOP('',(#4881,#4882,#4883,#4884));
#1335=EDGE_LOOP('',(#4885,#4886,#4887,#4888));
#1336=EDGE_LOOP('',(#4889));
#1337=EDGE_LOOP('',(#4890));
#1338=EDGE_LOOP('',(#4891,#4892,#4893,#4894,#4895,#4896));
#1339=EDGE_LOOP('',(#4897,#4898,#4899,#4900));
#1340=EDGE_LOOP('',(#4901,#4902,#4903,#4904,#4905,#4906));
#1341=EDGE_LOOP('',(#4907));
#1342=EDGE_LOOP('',(#4908));
#1343=EDGE_LOOP('',(#4909,#4910,#4911,#4912));
#1344=EDGE_LOOP('',(#4913));
#1345=EDGE_LOOP('',(#4914));
#1346=EDGE_LOOP('',(#4915,#4916,#4917,#4918));
#1347=EDGE_LOOP('',(#4919,#4920,#4921,#4922));
#1348=EDGE_LOOP('',(#4923));
#1349=EDGE_LOOP('',(#4924));
#1350=EDGE_LOOP('',(#4925));
#1351=EDGE_LOOP('',(#4926));
#1352=EDGE_LOOP('',(#4927));
#1353=EDGE_LOOP('',(#4928));
#1354=EDGE_LOOP('',(#4929));
#1355=EDGE_LOOP('',(#4930));
#1356=EDGE_LOOP('',(#4931));
#1357=EDGE_LOOP('',(#4932,#4933,#4934,#4935,#4936,#4937,#4938,#4939));
#1358=EDGE_LOOP('',(#4940));
#1359=EDGE_LOOP('',(#4941));
#1360=EDGE_LOOP('',(#4942));
#1361=EDGE_LOOP('',(#4943));
#1362=EDGE_LOOP('',(#4944));
#1363=EDGE_LOOP('',(#4945));
#1364=EDGE_LOOP('',(#4946));
#1365=EDGE_LOOP('',(#4947));
#1366=EDGE_LOOP('',(#4948));
#1367=EDGE_LOOP('',(#4949,#4950,#4951,#4952));
#1368=EDGE_LOOP('',(#4953,#4954,#4955,#4956));
#1369=EDGE_LOOP('',(#4957,#4958,#4959,#4960));
#1370=EDGE_LOOP('',(#4961,#4962,#4963,#4964));
#1371=EDGE_LOOP('',(#4965,#4966,#4967,#4968));
#1372=EDGE_LOOP('',(#4969,#4970,#4971,#4972));
#1373=EDGE_LOOP('',(#4973,#4974,#4975,#4976));
#1374=EDGE_LOOP('',(#4977,#4978,#4979,#4980));
#1375=EDGE_LOOP('',(#4981,#4982,#4983,#4984,#4985,#4986,#4987,#4988));
#1376=EDGE_LOOP('',(#4989,#4990,#4991,#4992));
#1377=EDGE_LOOP('',(#4993,#4994,#4995,#4996));
#1378=EDGE_LOOP('',(#4997,#4998,#4999,#5000,#5001,#5002,#5003,#5004));
#1379=EDGE_LOOP('',(#5005,#5006,#5007,#5008));
#1380=EDGE_LOOP('',(#5009,#5010,#5011,#5012));
#1381=EDGE_LOOP('',(#5013,#5014,#5015,#5016));
#1382=EDGE_LOOP('',(#5017,#5018,#5019,#5020));
#1383=EDGE_LOOP('',(#5021,#5022,#5023,#5024));
#1384=EDGE_LOOP('',(#5025,#5026,#5027,#5028,#5029,#5030,#5031,#5032));
#1385=EDGE_LOOP('',(#5033));
#1386=EDGE_LOOP('',(#5034));
#1387=EDGE_LOOP('',(#5035));
#1388=EDGE_LOOP('',(#5036));
#1389=EDGE_LOOP('',(#5037));
#1390=EDGE_LOOP('',(#5038));
#1391=EDGE_LOOP('',(#5039));
#1392=EDGE_LOOP('',(#5040));
#1393=EDGE_LOOP('',(#5041));
#1394=EDGE_LOOP('',(#5042,#5043,#5044,#5045));
#1395=EDGE_LOOP('',(#5046));
#1396=EDGE_LOOP('',(#5047));
#1397=EDGE_LOOP('',(#5048));
#1398=EDGE_LOOP('',(#5049));
#1399=EDGE_LOOP('',(#5050));
#1400=EDGE_LOOP('',(#5051));
#1401=EDGE_LOOP('',(#5052));
#1402=EDGE_LOOP('',(#5053));
#1403=EDGE_LOOP('',(#5054));
#1404=EDGE_LOOP('',(#5055,#5056,#5057,#5058));
#1405=EDGE_LOOP('',(#5059,#5060,#5061,#5062));
#1406=EDGE_LOOP('',(#5063,#5064,#5065,#5066));
#1407=EDGE_LOOP('',(#5067,#5068,#5069,#5070));
#1408=EDGE_LOOP('',(#5071,#5072,#5073,#5074));
#1409=EDGE_LOOP('',(#5075,#5076,#5077,#5078));
#1410=EDGE_LOOP('',(#5079,#5080,#5081,#5082));
#1411=EDGE_LOOP('',(#5083,#5084,#5085,#5086));
#1412=EDGE_LOOP('',(#5087,#5088,#5089,#5090));
#1413=EDGE_LOOP('',(#5091,#5092,#5093,#5094));
#1414=EDGE_LOOP('',(#5095,#5096,#5097,#5098));
#1415=EDGE_LOOP('',(#5099));
#1416=EDGE_LOOP('',(#5100));
#1417=EDGE_LOOP('',(#5101));
#1418=EDGE_LOOP('',(#5102,#5103,#5104,#5105));
#1419=EDGE_LOOP('',(#5106));
#1420=EDGE_LOOP('',(#5107));
#1421=EDGE_LOOP('',(#5108,#5109,#5110,#5111));
#1422=EDGE_LOOP('',(#5112));
#1423=EDGE_LOOP('',(#5113,#5114,#5115,#5116));
#1424=EDGE_LOOP('',(#5117,#5118,#5119,#5120));
#1425=EDGE_LOOP('',(#5121));
#1426=EDGE_LOOP('',(#5122));
#1427=EDGE_LOOP('',(#5123,#5124,#5125,#5126));
#1428=EDGE_LOOP('',(#5127,#5128,#5129,#5130));
#1429=EDGE_LOOP('',(#5131,#5132,#5133,#5134));
#1430=EDGE_LOOP('',(#5135,#5136,#5137,#5138));
#1431=EDGE_LOOP('',(#5139,#5140,#5141,#5142));
#1432=EDGE_LOOP('',(#5143,#5144,#5145,#5146));
#1433=EDGE_LOOP('',(#5147));
#1434=EDGE_LOOP('',(#5148));
#1435=EDGE_LOOP('',(#5149,#5150,#5151,#5152));
#1436=EDGE_LOOP('',(#5153,#5154,#5155,#5156));
#1437=EDGE_LOOP('',(#5157,#5158,#5159,#5160));
#1438=EDGE_LOOP('',(#5161,#5162,#5163,#5164));
#1439=EDGE_LOOP('',(#5165,#5166,#5167,#5168));
#1440=EDGE_LOOP('',(#5169,#5170,#5171,#5172));
#1441=EDGE_LOOP('',(#5173,#5174,#5175,#5176));
#1442=EDGE_LOOP('',(#5177,#5178,#5179,#5180));
#1443=EDGE_LOOP('',(#5181));
#1444=EDGE_LOOP('',(#5182));
#1445=EDGE_LOOP('',(#5183,#5184,#5185,#5186));
#1446=EDGE_LOOP('',(#5187,#5188,#5189,#5190));
#1447=EDGE_LOOP('',(#5191,#5192,#5193,#5194));
#1448=EDGE_LOOP('',(#5195,#5196,#5197,#5198));
#1449=EDGE_LOOP('',(#5199,#5200,#5201,#5202));
#1450=EDGE_LOOP('',(#5203,#5204,#5205,#5206));
#1451=EDGE_LOOP('',(#5207));
#1452=EDGE_LOOP('',(#5208));
#1453=EDGE_LOOP('',(#5209,#5210,#5211,#5212));
#1454=EDGE_LOOP('',(#5213,#5214,#5215,#5216,#5217,#5218));
#1455=EDGE_LOOP('',(#5219));
#1456=EDGE_LOOP('',(#5220));
#1457=EDGE_LOOP('',(#5221,#5222,#5223,#5224,#5225,#5226,#5227,#5228));
#1458=EDGE_LOOP('',(#5229,#5230,#5231,#5232));
#1459=EDGE_LOOP('',(#5233,#5234,#5235,#5236));
#1460=EDGE_LOOP('',(#5237,#5238,#5239,#5240));
#1461=EDGE_LOOP('',(#5241,#5242,#5243,#5244,#5245,#5246,#5247,#5248));
#1462=EDGE_LOOP('',(#5249,#5250,#5251,#5252));
#1463=EDGE_LOOP('',(#5253));
#1464=EDGE_LOOP('',(#5254));
#1465=EDGE_LOOP('',(#5255,#5256,#5257,#5258));
#1466=EDGE_LOOP('',(#5259,#5260,#5261,#5262,#5263,#5264));
#1467=EDGE_LOOP('',(#5265));
#1468=EDGE_LOOP('',(#5266));
#1469=EDGE_LOOP('',(#5267,#5268,#5269,#5270));
#1470=EDGE_LOOP('',(#5271,#5272,#5273,#5274));
#1471=EDGE_LOOP('',(#5275));
#1472=EDGE_LOOP('',(#5276));
#1473=EDGE_LOOP('',(#5277,#5278,#5279,#5280));
#1474=EDGE_LOOP('',(#5281,#5282,#5283,#5284));
#1475=EDGE_LOOP('',(#5285,#5286,#5287,#5288));
#1476=EDGE_LOOP('',(#5289,#5290,#5291,#5292));
#1477=EDGE_LOOP('',(#5293,#5294,#5295,#5296));
#1478=EDGE_LOOP('',(#5297,#5298,#5299,#5300));
#1479=EDGE_LOOP('',(#5301));
#1480=EDGE_LOOP('',(#5302));
#1481=EDGE_LOOP('',(#5303,#5304,#5305,#5306));
#1482=EDGE_LOOP('',(#5307,#5308,#5309,#5310));
#1483=EDGE_LOOP('',(#5311,#5312,#5313,#5314));
#1484=EDGE_LOOP('',(#5315,#5316,#5317,#5318));
#1485=EDGE_LOOP('',(#5319,#5320,#5321,#5322));
#1486=EDGE_LOOP('',(#5323,#5324,#5325,#5326));
#1487=EDGE_LOOP('',(#5327));
#1488=EDGE_LOOP('',(#5328));
#1489=EDGE_LOOP('',(#5329,#5330,#5331,#5332));
#1490=EDGE_LOOP('',(#5333,#5334,#5335,#5336));
#1491=EDGE_LOOP('',(#5337));
#1492=EDGE_LOOP('',(#5338));
#1493=EDGE_LOOP('',(#5339,#5340,#5341,#5342));
#1494=EDGE_LOOP('',(#5343,#5344,#5345,#5346));
#1495=EDGE_LOOP('',(#5347,#5348,#5349,#5350));
#1496=EDGE_LOOP('',(#5351,#5352,#5353,#5354));
#1497=EDGE_LOOP('',(#5355,#5356,#5357,#5358));
#1498=EDGE_LOOP('',(#5359,#5360,#5361,#5362));
#1499=EDGE_LOOP('',(#5363));
#1500=EDGE_LOOP('',(#5364));
#1501=EDGE_LOOP('',(#5365,#5366));
#1502=EDGE_LOOP('',(#5367,#5368,#5369,#5370,#5371,#5372));
#1503=EDGE_LOOP('',(#5373,#5374));
#1504=EDGE_LOOP('',(#5375,#5376,#5377,#5378));
#1505=EDGE_LOOP('',(#5379));
#1506=EDGE_LOOP('',(#5380));
#1507=EDGE_LOOP('',(#5381,#5382,#5383,#5384));
#1508=EDGE_LOOP('',(#5385));
#1509=EDGE_LOOP('',(#5386));
#1510=EDGE_LOOP('',(#5387));
#1511=EDGE_LOOP('',(#5388));
#1512=EDGE_LOOP('',(#5389,#5390,#5391,#5392));
#1513=EDGE_LOOP('',(#5393,#5394));
#1514=EDGE_LOOP('',(#5395,#5396,#5397,#5398,#5399,#5400));
#1515=EDGE_LOOP('',(#5401,#5402));
#1516=EDGE_LOOP('',(#5403,#5404,#5405,#5406));
#1517=EDGE_LOOP('',(#5407));
#1518=EDGE_LOOP('',(#5408));
#1519=EDGE_LOOP('',(#5409,#5410,#5411,#5412));
#1520=EDGE_LOOP('',(#5413));
#1521=EDGE_LOOP('',(#5414));
#1522=EDGE_LOOP('',(#5415,#5416,#5417,#5418));
#1523=EDGE_LOOP('',(#5419));
#1524=EDGE_LOOP('',(#5420));
#1525=EDGE_LOOP('',(#5421));
#1526=EDGE_LOOP('',(#5422));
#1527=EDGE_LOOP('',(#5423));
#1528=EDGE_LOOP('',(#5424,#5425,#5426,#5427));
#1529=EDGE_LOOP('',(#5428,#5429,#5430,#5431));
#1530=EDGE_LOOP('',(#5432,#5433,#5434,#5435));
#1531=EDGE_LOOP('',(#5436,#5437,#5438,#5439));
#1532=EDGE_LOOP('',(#5440,#5441,#5442,#5443));
#1533=EDGE_LOOP('',(#5444,#5445,#5446,#5447));
#1534=EDGE_LOOP('',(#5448,#5449,#5450,#5451));
#1535=EDGE_LOOP('',(#5452,#5453,#5454,#5455));
#1536=EDGE_LOOP('',(#5456,#5457,#5458,#5459));
#1537=EDGE_LOOP('',(#5460,#5461,#5462,#5463));
#1538=EDGE_LOOP('',(#5464));
#1539=EDGE_LOOP('',(#5465));
#1540=EDGE_LOOP('',(#5466));
#1541=EDGE_LOOP('',(#5467));
#1542=EDGE_LOOP('',(#5468));
#1543=EDGE_LOOP('',(#5469,#5470,#5471,#5472));
#1544=EDGE_LOOP('',(#5473));
#1545=EDGE_LOOP('',(#5474));
#1546=EDGE_LOOP('',(#5475));
#1547=EDGE_LOOP('',(#5476));
#1548=EDGE_LOOP('',(#5477,#5478,#5479,#5480));
#1549=EDGE_LOOP('',(#5481,#5482,#5483,#5484));
#1550=EDGE_LOOP('',(#5485));
#1551=EDGE_LOOP('',(#5486));
#1552=EDGE_LOOP('',(#5487));
#1553=EDGE_LOOP('',(#5488));
#1554=EDGE_LOOP('',(#5489,#5490,#5491,#5492));
#1555=EDGE_LOOP('',(#5493,#5494,#5495,#5496));
#1556=EDGE_LOOP('',(#5497));
#1557=EDGE_LOOP('',(#5498));
#1558=LINE('',#9331,#1917);
#1559=LINE('',#9337,#1918);
#1560=LINE('',#9344,#1919);
#1561=LINE('',#9349,#1920);
#1562=LINE('',#9354,#1921);
#1563=LINE('',#9357,#1922);
#1564=LINE('',#9368,#1923);
#1565=LINE('',#9371,#1924);
#1566=LINE('',#9406,#1925);
#1567=LINE('',#9408,#1926);
#1568=LINE('',#9410,#1927);
#1569=LINE('',#9412,#1928);
#1570=LINE('',#9414,#1929);
#1571=LINE('',#9416,#1930);
#1572=LINE('',#9418,#1931);
#1573=LINE('',#9421,#1932);
#1574=LINE('',#9443,#1933);
#1575=LINE('',#9455,#1934);
#1576=LINE('',#9475,#1935);
#1577=LINE('',#9478,#1936);
#1578=LINE('',#9494,#1937);
#1579=LINE('',#9510,#1938);
#1580=LINE('',#9536,#1939);
#1581=LINE('',#9548,#1940);
#1582=LINE('',#9568,#1941);
#1583=LINE('',#9571,#1942);
#1584=LINE('',#9587,#1943);
#1585=LINE('',#9603,#1944);
#1586=LINE('',#9616,#1945);
#1587=LINE('',#9623,#1946);
#1588=LINE('',#9628,#1947);
#1589=LINE('',#9633,#1948);
#1590=LINE('',#9636,#1949);
#1591=LINE('',#9647,#1950);
#1592=LINE('',#9650,#1951);
#1593=LINE('',#9685,#1952);
#1594=LINE('',#9687,#1953);
#1595=LINE('',#9689,#1954);
#1596=LINE('',#9691,#1955);
#1597=LINE('',#9693,#1956);
#1598=LINE('',#9695,#1957);
#1599=LINE('',#9697,#1958);
#1600=LINE('',#9700,#1959);
#1601=LINE('',#9709,#1960);
#1602=LINE('',#9716,#1961);
#1603=LINE('',#9719,#1962);
#1604=LINE('',#9722,#1963);
#1605=LINE('',#9724,#1964);
#1606=LINE('',#9725,#1965);
#1607=LINE('',#9728,#1966);
#1608=LINE('',#9731,#1967);
#1609=LINE('',#9736,#1968);
#1610=LINE('',#9737,#1969);
#1611=LINE('',#9740,#1970);
#1612=LINE('',#9741,#1971);
#1613=LINE('',#9745,#1972);
#1614=LINE('',#9750,#1973);
#1615=LINE('',#9751,#1974);
#1616=LINE('',#9753,#1975);
#1617=LINE('',#9754,#1976);
#1618=LINE('',#9756,#1977);
#1619=LINE('',#9757,#1978);
#1620=LINE('',#9760,#1979);
#1621=LINE('',#9761,#1980);
#1622=LINE('',#9763,#1981);
#1623=LINE('',#9767,#1982);
#1624=LINE('',#9771,#1983);
#1625=LINE('',#9773,#1984);
#1626=LINE('',#9780,#1985);
#1627=LINE('',#9785,#1986);
#1628=LINE('',#9787,#1987);
#1629=LINE('',#9789,#1988);
#1630=LINE('',#9790,#1989);
#1631=LINE('',#9802,#1990);
#1632=LINE('',#9804,#1991);
#1633=LINE('',#9806,#1992);
#1634=LINE('',#9807,#1993);
#1635=LINE('',#9817,#1994);
#1636=LINE('',#9819,#1995);
#1637=LINE('',#9821,#1996);
#1638=LINE('',#9823,#1997);
#1639=LINE('',#9825,#1998);
#1640=LINE('',#9826,#1999);
#1641=LINE('',#9828,#2000);
#1642=LINE('',#9830,#2001);
#1643=LINE('',#9850,#2002);
#1644=LINE('',#9862,#2003);
#1645=LINE('',#9882,#2004);
#1646=LINE('',#9885,#2005);
#1647=LINE('',#9901,#2006);
#1648=LINE('',#9917,#2007);
#1649=LINE('',#9930,#2008);
#1650=LINE('',#9940,#2009);
#1651=LINE('',#9942,#2010);
#1652=LINE('',#9955,#2011);
#1653=LINE('',#9959,#2012);
#1654=LINE('',#9963,#2013);
#1655=LINE('',#9967,#2014);
#1656=LINE('',#9971,#2015);
#1657=LINE('',#9974,#2016);
#1658=LINE('',#9976,#2017);
#1659=LINE('',#9977,#2018);
#1660=LINE('',#9980,#2019);
#1661=LINE('',#9981,#2020);
#1662=LINE('',#9984,#2021);
#1663=LINE('',#10007,#2022);
#1664=LINE('',#10019,#2023);
#1665=LINE('',#10039,#2024);
#1666=LINE('',#10042,#2025);
#1667=LINE('',#10058,#2026);
#1668=LINE('',#10074,#2027);
#1669=LINE('',#10088,#2028);
#1670=LINE('',#10097,#2029);
#1671=LINE('',#10111,#2030);
#1672=LINE('',#10120,#2031);
#1673=LINE('',#10123,#2032);
#1674=LINE('',#10124,#2033);
#1675=LINE('',#10127,#2034);
#1676=LINE('',#10128,#2035);
#1677=LINE('',#10130,#2036);
#1678=LINE('',#10133,#2037);
#1679=LINE('',#10134,#2038);
#1680=LINE('',#10137,#2039);
#1681=LINE('',#10138,#2040);
#1682=LINE('',#10141,#2041);
#1683=LINE('',#10143,#2042);
#1684=LINE('',#10144,#2043);
#1685=LINE('',#10147,#2044);
#1686=LINE('',#10148,#2045);
#1687=LINE('',#10151,#2046);
#1688=LINE('',#10152,#2047);
#1689=LINE('',#10154,#2048);
#1690=LINE('',#10161,#2049);
#1691=LINE('',#10170,#2050);
#1692=LINE('',#10184,#2051);
#1693=LINE('',#10193,#2052);
#1694=LINE('',#10196,#2053);
#1695=LINE('',#10197,#2054);
#1696=LINE('',#10200,#2055);
#1697=LINE('',#10201,#2056);
#1698=LINE('',#10203,#2057);
#1699=LINE('',#10206,#2058);
#1700=LINE('',#10207,#2059);
#1701=LINE('',#10210,#2060);
#1702=LINE('',#10211,#2061);
#1703=LINE('',#10214,#2062);
#1704=LINE('',#10216,#2063);
#1705=LINE('',#10217,#2064);
#1706=LINE('',#10220,#2065);
#1707=LINE('',#10221,#2066);
#1708=LINE('',#10224,#2067);
#1709=LINE('',#10225,#2068);
#1710=LINE('',#10227,#2069);
#1711=LINE('',#10241,#2070);
#1712=LINE('',#10250,#2071);
#1713=LINE('',#10253,#2072);
#1714=LINE('',#10254,#2073);
#1715=LINE('',#10257,#2074);
#1716=LINE('',#10258,#2075);
#1717=LINE('',#10260,#2076);
#1718=LINE('',#10263,#2077);
#1719=LINE('',#10264,#2078);
#1720=LINE('',#10267,#2079);
#1721=LINE('',#10268,#2080);
#1722=LINE('',#10271,#2081);
#1723=LINE('',#10273,#2082);
#1724=LINE('',#10274,#2083);
#1725=LINE('',#10277,#2084);
#1726=LINE('',#10278,#2085);
#1727=LINE('',#10281,#2086);
#1728=LINE('',#10282,#2087);
#1729=LINE('',#10284,#2088);
#1730=LINE('',#10291,#2089);
#1731=LINE('',#10300,#2090);
#1732=LINE('',#10308,#2091);
#1733=LINE('',#10317,#2092);
#1734=LINE('',#10326,#2093);
#1735=LINE('',#10333,#2094);
#1736=LINE('',#10339,#2095);
#1737=LINE('',#10345,#2096);
#1738=LINE('',#10349,#2097);
#1739=LINE('',#10351,#2098);
#1740=LINE('',#10354,#2099);
#1741=LINE('',#10369,#2100);
#1742=LINE('',#10374,#2101);
#1743=LINE('',#10376,#2102);
#1744=LINE('',#10378,#2103);
#1745=LINE('',#10379,#2104);
#1746=LINE('',#10399,#2105);
#1747=LINE('',#10401,#2106);
#1748=LINE('',#10403,#2107);
#1749=LINE('',#10405,#2108);
#1750=LINE('',#10407,#2109);
#1751=LINE('',#10409,#2110);
#1752=LINE('',#10411,#2111);
#1753=LINE('',#10412,#2112);
#1754=LINE('',#10430,#2113);
#1755=LINE('',#10432,#2114);
#1756=LINE('',#10434,#2115);
#1757=LINE('',#10436,#2116);
#1758=LINE('',#10438,#2117);
#1759=LINE('',#10440,#2118);
#1760=LINE('',#10442,#2119);
#1761=LINE('',#10444,#2120);
#1762=LINE('',#10448,#2121);
#1763=LINE('',#10450,#2122);
#1764=LINE('',#10452,#2123);
#1765=LINE('',#10453,#2124);
#1766=LINE('',#10454,#2125);
#1767=LINE('',#10455,#2126);
#1768=LINE('',#10457,#2127);
#1769=LINE('',#10459,#2128);
#1770=LINE('',#10462,#2129);
#1771=LINE('',#10464,#2130);
#1772=LINE('',#10466,#2131);
#1773=LINE('',#10467,#2132);
#1774=LINE('',#10470,#2133);
#1775=LINE('',#10471,#2134);
#1776=LINE('',#10474,#2135);
#1777=LINE('',#10475,#2136);
#1778=LINE('',#10478,#2137);
#1779=LINE('',#10479,#2138);
#1780=LINE('',#10481,#2139);
#1781=LINE('',#10485,#2140);
#1782=LINE('',#10486,#2141);
#1783=LINE('',#10487,#2142);
#1784=LINE('',#10489,#2143);
#1785=LINE('',#10509,#2144);
#1786=LINE('',#10530,#2145);
#1787=LINE('',#10532,#2146);
#1788=LINE('',#10534,#2147);
#1789=LINE('',#10536,#2148);
#1790=LINE('',#10538,#2149);
#1791=LINE('',#10540,#2150);
#1792=LINE('',#10542,#2151);
#1793=LINE('',#10544,#2152);
#1794=LINE('',#10546,#2153);
#1795=LINE('',#10552,#2154);
#1796=LINE('',#10561,#2155);
#1797=LINE('',#10568,#2156);
#1798=LINE('',#10576,#2157);
#1799=LINE('',#10581,#2158);
#1800=LINE('',#10583,#2159);
#1801=LINE('',#10586,#2160);
#1802=LINE('',#10591,#2161);
#1803=LINE('',#10595,#2162);
#1804=LINE('',#10597,#2163);
#1805=LINE('',#10598,#2164);
#1806=LINE('',#10601,#2165);
#1807=LINE('',#10605,#2166);
#1808=LINE('',#10606,#2167);
#1809=LINE('',#10608,#2168);
#1810=LINE('',#10614,#2169);
#1811=LINE('',#10616,#2170);
#1812=LINE('',#10618,#2171);
#1813=LINE('',#10619,#2172);
#1814=LINE('',#10622,#2173);
#1815=LINE('',#10624,#2174);
#1816=LINE('',#10625,#2175);
#1817=LINE('',#10628,#2176);
#1818=LINE('',#10629,#2177);
#1819=LINE('',#10632,#2178);
#1820=LINE('',#10633,#2179);
#1821=LINE('',#10635,#2180);
#1822=LINE('',#10642,#2181);
#1823=LINE('',#10647,#2182);
#1824=LINE('',#10649,#2183);
#1825=LINE('',#10652,#2184);
#1826=LINE('',#10657,#2185);
#1827=LINE('',#10661,#2186);
#1828=LINE('',#10663,#2187);
#1829=LINE('',#10664,#2188);
#1830=LINE('',#10667,#2189);
#1831=LINE('',#10671,#2190);
#1832=LINE('',#10672,#2191);
#1833=LINE('',#10674,#2192);
#1834=LINE('',#10681,#2193);
#1835=LINE('',#10686,#2194);
#1836=LINE('',#10688,#2195);
#1837=LINE('',#10690,#2196);
#1838=LINE('',#10692,#2197);
#1839=LINE('',#10694,#2198);
#1840=LINE('',#10695,#2199);
#1841=LINE('',#10703,#2200);
#1842=LINE('',#10705,#2201);
#1843=LINE('',#10707,#2202);
#1844=LINE('',#10709,#2203);
#1845=LINE('',#10710,#2204);
#1846=LINE('',#10712,#2205);
#1847=LINE('',#10713,#2206);
#1848=LINE('',#10716,#2207);
#1849=LINE('',#10717,#2208);
#1850=LINE('',#10720,#2209);
#1851=LINE('',#10721,#2210);
#1852=LINE('',#10724,#2211);
#1853=LINE('',#10725,#2212);
#1854=LINE('',#10729,#2213);
#1855=LINE('',#10731,#2214);
#1856=LINE('',#10733,#2215);
#1857=LINE('',#10735,#2216);
#1858=LINE('',#10736,#2217);
#1859=LINE('',#10737,#2218);
#1860=LINE('',#10739,#2219);
#1861=LINE('',#10740,#2220);
#1862=LINE('',#10744,#2221);
#1863=LINE('',#10749,#2222);
#1864=LINE('',#10751,#2223);
#1865=LINE('',#10758,#2224);
#1866=LINE('',#10760,#2225);
#1867=LINE('',#10762,#2226);
#1868=LINE('',#10768,#2227);
#1869=LINE('',#10773,#2228);
#1870=LINE('',#10775,#2229);
#1871=LINE('',#10778,#2230);
#1872=LINE('',#10783,#2231);
#1873=LINE('',#10787,#2232);
#1874=LINE('',#10789,#2233);
#1875=LINE('',#10790,#2234);
#1876=LINE('',#10793,#2235);
#1877=LINE('',#10797,#2236);
#1878=LINE('',#10798,#2237);
#1879=LINE('',#10800,#2238);
#1880=LINE('',#10807,#2239);
#1881=LINE('',#10812,#2240);
#1882=LINE('',#10814,#2241);
#1883=LINE('',#10817,#2242);
#1884=LINE('',#10822,#2243);
#1885=LINE('',#10826,#2244);
#1886=LINE('',#10828,#2245);
#1887=LINE('',#10829,#2246);
#1888=LINE('',#10832,#2247);
#1889=LINE('',#10836,#2248);
#1890=LINE('',#10837,#2249);
#1891=LINE('',#10839,#2250);
#1892=LINE('',#10856,#2251);
#1893=LINE('',#10866,#2252);
#1894=LINE('',#10875,#2253);
#1895=LINE('',#10884,#2254);
#1896=LINE('',#10893,#2255);
#1897=LINE('',#10903,#2256);
#1898=LINE('',#10917,#2257);
#1899=LINE('',#10925,#2258);
#1900=LINE('',#10927,#2259);
#1901=LINE('',#10942,#2260);
#1902=LINE('',#10946,#2261);
#1903=LINE('',#10950,#2262);
#1904=LINE('',#10954,#2263);
#1905=LINE('',#10958,#2264);
#1906=LINE('',#10961,#2265);
#1907=LINE('',#10963,#2266);
#1908=LINE('',#10964,#2267);
#1909=LINE('',#10968,#2268);
#1910=LINE('',#10971,#2269);
#1911=LINE('',#10974,#2270);
#1912=LINE('',#10982,#2271);
#1913=LINE('',#10991,#2272);
#1914=LINE('',#10997,#2273);
#1915=LINE('',#11006,#2274);
#1916=LINE('',#11012,#2275);
#1917=VECTOR('',#7268,0.00749999975240882);
#1918=VECTOR('',#7275,0.042);
#1919=VECTOR('',#7284,1.);
#1920=VECTOR('',#7289,1.);
#1921=VECTOR('',#7296,0.05);
#1922=VECTOR('',#7299,0.05);
#1923=VECTOR('',#7314,0.04);
#1924=VECTOR('',#7317,0.04);
#1925=VECTOR('',#7356,0.028);
#1926=VECTOR('',#7359,0.0025);
#1927=VECTOR('',#7362,0.0025);
#1928=VECTOR('',#7365,0.0025);
#1929=VECTOR('',#7368,0.0025);
#1930=VECTOR('',#7371,0.0025);
#1931=VECTOR('',#7374,0.0025);
#1932=VECTOR('',#7377,0.028);
#1933=VECTOR('',#7408,0.026);
#1934=VECTOR('',#7423,0.02045);
#1935=VECTOR('',#7450,0.02045);
#1936=VECTOR('',#7453,0.01305);
#1937=VECTOR('',#7474,0.01305);
#1938=VECTOR('',#7495,0.0075);
#1939=VECTOR('',#7532,0.026);
#1940=VECTOR('',#7547,0.02045);
#1941=VECTOR('',#7574,0.02045);
#1942=VECTOR('',#7577,0.01305);
#1943=VECTOR('',#7598,0.01305);
#1944=VECTOR('',#7619,0.0075);
#1945=VECTOR('',#7638,0.042);
#1946=VECTOR('',#7647,1.);
#1947=VECTOR('',#7652,1.);
#1948=VECTOR('',#7659,0.05);
#1949=VECTOR('',#7662,0.05);
#1950=VECTOR('',#7677,0.04);
#1951=VECTOR('',#7680,0.04);
#1952=VECTOR('',#7719,0.028);
#1953=VECTOR('',#7722,0.0025);
#1954=VECTOR('',#7725,0.0025);
#1955=VECTOR('',#7728,0.0025);
#1956=VECTOR('',#7731,0.0025);
#1957=VECTOR('',#7734,0.0025);
#1958=VECTOR('',#7737,0.0025);
#1959=VECTOR('',#7740,0.028);
#1960=VECTOR('',#7753,0.025);
#1961=VECTOR('',#7760,0.01);
#1962=VECTOR('',#7763,0.01);
#1963=VECTOR('',#7766,0.01);
#1964=VECTOR('',#7767,0.01);
#1965=VECTOR('',#7768,0.01);
#1966=VECTOR('',#7771,0.01);
#1967=VECTOR('',#7774,0.01);
#1968=VECTOR('',#7779,0.01);
#1969=VECTOR('',#7780,0.01);
#1970=VECTOR('',#7783,0.01);
#1971=VECTOR('',#7784,0.01);
#1972=VECTOR('',#7787,0.01);
#1973=VECTOR('',#7794,0.01);
#1974=VECTOR('',#7795,0.01);
#1975=VECTOR('',#7798,0.01);
#1976=VECTOR('',#7799,0.01);
#1977=VECTOR('',#7802,0.01);
#1978=VECTOR('',#7803,0.01);
#1979=VECTOR('',#7806,0.01);
#1980=VECTOR('',#7807,0.01);
#1981=VECTOR('',#7810,0.01);
#1982=VECTOR('',#7815,0.01);
#1983=VECTOR('',#7822,0.01);
#1984=VECTOR('',#7825,0.01);
#1985=VECTOR('',#7834,0.005);
#1986=VECTOR('',#7839,0.01);
#1987=VECTOR('',#7840,0.01);
#1988=VECTOR('',#7841,0.01);
#1989=VECTOR('',#7842,0.01);
#1990=VECTOR('',#7853,0.01);
#1991=VECTOR('',#7854,0.01);
#1992=VECTOR('',#7855,0.01);
#1993=VECTOR('',#7856,0.01);
#1994=VECTOR('',#7867,0.005);
#1995=VECTOR('',#7870,0.005);
#1996=VECTOR('',#7873,0.025);
#1997=VECTOR('',#7876,0.005);
#1998=VECTOR('',#7879,0.01);
#1999=VECTOR('',#7880,0.01);
#2000=VECTOR('',#7883,0.01);
#2001=VECTOR('',#7886,0.01);
#2002=VECTOR('',#7913,0.026);
#2003=VECTOR('',#7928,0.02045);
#2004=VECTOR('',#7955,0.02045);
#2005=VECTOR('',#7958,0.01305);
#2006=VECTOR('',#7979,0.01305);
#2007=VECTOR('',#8000,0.0075);
#2008=VECTOR('',#8019,0.028);
#2009=VECTOR('',#8030,0.01);
#2010=VECTOR('',#8031,0.01);
#2011=VECTOR('',#8046,0.025);
#2012=VECTOR('',#8051,0.0049999999999998);
#2013=VECTOR('',#8056,0.005);
#2014=VECTOR('',#8061,0.0049999999999998);
#2015=VECTOR('',#8066,0.005);
#2016=VECTOR('',#8069,0.01);
#2017=VECTOR('',#8070,0.01);
#2018=VECTOR('',#8071,0.01);
#2019=VECTOR('',#8074,0.01);
#2020=VECTOR('',#8075,0.01);
#2021=VECTOR('',#8078,0.01);
#2022=VECTOR('',#8111,0.026);
#2023=VECTOR('',#8126,0.02045);
#2024=VECTOR('',#8153,0.02045);
#2025=VECTOR('',#8156,0.01305);
#2026=VECTOR('',#8177,0.01305);
#2027=VECTOR('',#8198,0.0075);
#2028=VECTOR('',#8219,0.00799999973819874);
#2029=VECTOR('',#8232,0.00999999988959839);
#2030=VECTOR('',#8247,0.00799999961340774);
#2031=VECTOR('',#8260,0.01);
#2032=VECTOR('',#8263,0.01);
#2033=VECTOR('',#8264,0.01);
#2034=VECTOR('',#8267,0.01);
#2035=VECTOR('',#8268,0.01);
#2036=VECTOR('',#8271,0.01);
#2037=VECTOR('',#8274,0.01);
#2038=VECTOR('',#8275,0.01);
#2039=VECTOR('',#8278,0.01);
#2040=VECTOR('',#8279,0.01);
#2041=VECTOR('',#8282,0.01);
#2042=VECTOR('',#8283,0.01);
#2043=VECTOR('',#8284,0.01);
#2044=VECTOR('',#8287,0.01);
#2045=VECTOR('',#8288,0.01);
#2046=VECTOR('',#8291,0.01);
#2047=VECTOR('',#8292,0.01);
#2048=VECTOR('',#8295,0.01);
#2049=VECTOR('',#8304,0.00799999959059736);
#2050=VECTOR('',#8317,0.0099999996557502);
#2051=VECTOR('',#8332,0.00799999974118007);
#2052=VECTOR('',#8345,0.01);
#2053=VECTOR('',#8348,0.01);
#2054=VECTOR('',#8349,0.01);
#2055=VECTOR('',#8352,0.01);
#2056=VECTOR('',#8353,0.01);
#2057=VECTOR('',#8356,0.01);
#2058=VECTOR('',#8359,0.01);
#2059=VECTOR('',#8360,0.01);
#2060=VECTOR('',#8363,0.01);
#2061=VECTOR('',#8364,0.01);
#2062=VECTOR('',#8367,0.01);
#2063=VECTOR('',#8368,0.01);
#2064=VECTOR('',#8369,0.01);
#2065=VECTOR('',#8372,0.01);
#2066=VECTOR('',#8373,0.01);
#2067=VECTOR('',#8376,0.01);
#2068=VECTOR('',#8377,0.01);
#2069=VECTOR('',#8380,0.01);
#2070=VECTOR('',#8395,0.0079999999576051);
#2071=VECTOR('',#8408,0.01);
#2072=VECTOR('',#8411,0.01);
#2073=VECTOR('',#8412,0.01);
#2074=VECTOR('',#8415,0.01);
#2075=VECTOR('',#8416,0.01);
#2076=VECTOR('',#8419,0.01);
#2077=VECTOR('',#8422,0.01);
#2078=VECTOR('',#8423,0.01);
#2079=VECTOR('',#8426,0.01);
#2080=VECTOR('',#8427,0.01);
#2081=VECTOR('',#8430,0.01);
#2082=VECTOR('',#8431,0.01);
#2083=VECTOR('',#8432,0.01);
#2084=VECTOR('',#8435,0.01);
#2085=VECTOR('',#8436,0.01);
#2086=VECTOR('',#8439,0.01);
#2087=VECTOR('',#8440,0.01);
#2088=VECTOR('',#8443,0.01);
#2089=VECTOR('',#8452,0.00799999974106502);
#2090=VECTOR('',#8465,0.00999999987547767);
#2091=VECTOR('',#8474,0.00749999975240883);
#2092=VECTOR('',#8485,0.00749999975240883);
#2093=VECTOR('',#8494,0.00749999975240883);
#2094=VECTOR('',#8503,0.00749999975240883);
#2095=VECTOR('',#8510,0.00749999975240883);
#2096=VECTOR('',#8519,0.0075);
#2097=VECTOR('',#8524,0.015);
#2098=VECTOR('',#8527,0.0075);
#2099=VECTOR('',#8532,0.0075);
#2100=VECTOR('',#8557,0.01);
#2101=VECTOR('',#8562,0.01);
#2102=VECTOR('',#8563,0.01);
#2103=VECTOR('',#8564,0.01);
#2104=VECTOR('',#8565,0.01);
#2105=VECTOR('',#8584,0.01);
#2106=VECTOR('',#8585,0.01);
#2107=VECTOR('',#8586,0.01);
#2108=VECTOR('',#8587,0.01);
#2109=VECTOR('',#8588,0.01);
#2110=VECTOR('',#8589,0.01);
#2111=VECTOR('',#8590,0.01);
#2112=VECTOR('',#8591,0.01);
#2113=VECTOR('',#8610,0.00499999999997557);
#2114=VECTOR('',#8613,0.00499999999997558);
#2115=VECTOR('',#8616,0.00500000000000013);
#2116=VECTOR('',#8619,0.005);
#2117=VECTOR('',#8622,0.005);
#2118=VECTOR('',#8625,0.00500000000000013);
#2119=VECTOR('',#8628,0.00499999999997557);
#2120=VECTOR('',#8631,0.00499999999997558);
#2121=VECTOR('',#8634,0.01);
#2122=VECTOR('',#8635,0.01);
#2123=VECTOR('',#8636,0.01);
#2124=VECTOR('',#8637,0.01);
#2125=VECTOR('',#8638,0.01);
#2126=VECTOR('',#8639,0.01);
#2127=VECTOR('',#8642,0.01);
#2128=VECTOR('',#8645,0.01);
#2129=VECTOR('',#8648,0.01);
#2130=VECTOR('',#8649,0.01);
#2131=VECTOR('',#8650,0.01);
#2132=VECTOR('',#8651,0.01);
#2133=VECTOR('',#8654,0.01);
#2134=VECTOR('',#8655,0.01);
#2135=VECTOR('',#8658,0.01);
#2136=VECTOR('',#8659,0.01);
#2137=VECTOR('',#8662,0.01);
#2138=VECTOR('',#8663,0.01);
#2139=VECTOR('',#8666,0.01);
#2140=VECTOR('',#8669,0.01);
#2141=VECTOR('',#8670,0.01);
#2142=VECTOR('',#8671,0.01);
#2143=VECTOR('',#8674,0.01);
#2144=VECTOR('',#8695,0.01);
#2145=VECTOR('',#8718,0.005);
#2146=VECTOR('',#8721,0.005);
#2147=VECTOR('',#8724,0.00500000000000013);
#2148=VECTOR('',#8727,0.005);
#2149=VECTOR('',#8730,0.005);
#2150=VECTOR('',#8733,0.00500000000000013);
#2151=VECTOR('',#8736,0.005);
#2152=VECTOR('',#8739,0.005);
#2153=VECTOR('',#8742,0.01);
#2154=VECTOR('',#8749,0.003);
#2155=VECTOR('',#8762,0.0125);
#2156=VECTOR('',#8771,0.003);
#2157=VECTOR('',#8782,0.00118970000000007);
#2158=VECTOR('',#8787,0.01);
#2159=VECTOR('',#8788,0.01);
#2160=VECTOR('',#8791,0.01);
#2161=VECTOR('',#8796,0.00118970100000004);
#2162=VECTOR('',#8801,0.01);
#2163=VECTOR('',#8802,0.01);
#2164=VECTOR('',#8803,0.01);
#2165=VECTOR('',#8806,0.01);
#2166=VECTOR('',#8811,0.01);
#2167=VECTOR('',#8812,0.01);
#2168=VECTOR('',#8815,0.01);
#2169=VECTOR('',#8822,0.01);
#2170=VECTOR('',#8823,0.01);
#2171=VECTOR('',#8824,0.01);
#2172=VECTOR('',#8825,0.01);
#2173=VECTOR('',#8828,0.01);
#2174=VECTOR('',#8829,0.01);
#2175=VECTOR('',#8830,0.01);
#2176=VECTOR('',#8833,0.01);
#2177=VECTOR('',#8834,0.01);
#2178=VECTOR('',#8837,0.01);
#2179=VECTOR('',#8838,0.01);
#2180=VECTOR('',#8841,0.01);
#2181=VECTOR('',#8850,0.00118970000000007);
#2182=VECTOR('',#8855,0.01);
#2183=VECTOR('',#8856,0.01);
#2184=VECTOR('',#8859,0.01);
#2185=VECTOR('',#8864,0.00118970100000004);
#2186=VECTOR('',#8869,0.01);
#2187=VECTOR('',#8870,0.01);
#2188=VECTOR('',#8871,0.01);
#2189=VECTOR('',#8874,0.01);
#2190=VECTOR('',#8879,0.01);
#2191=VECTOR('',#8880,0.01);
#2192=VECTOR('',#8883,0.01);
#2193=VECTOR('',#8892,0.00118970099999992);
#2194=VECTOR('',#8897,0.01);
#2195=VECTOR('',#8898,0.01);
#2196=VECTOR('',#8899,0.01);
#2197=VECTOR('',#8900,0.01);
#2198=VECTOR('',#8901,0.01);
#2199=VECTOR('',#8902,0.01);
#2200=VECTOR('',#8909,0.01);
#2201=VECTOR('',#8910,0.01);
#2202=VECTOR('',#8911,0.01);
#2203=VECTOR('',#8912,0.01);
#2204=VECTOR('',#8913,0.01);
#2205=VECTOR('',#8914,0.01);
#2206=VECTOR('',#8915,0.01);
#2207=VECTOR('',#8918,0.01);
#2208=VECTOR('',#8919,0.01);
#2209=VECTOR('',#8922,0.01);
#2210=VECTOR('',#8923,0.01);
#2211=VECTOR('',#8926,0.01);
#2212=VECTOR('',#8927,0.01);
#2213=VECTOR('',#8930,0.01);
#2214=VECTOR('',#8931,0.01);
#2215=VECTOR('',#8932,0.01);
#2216=VECTOR('',#8933,0.01);
#2217=VECTOR('',#8934,0.01);
#2218=VECTOR('',#8935,0.01);
#2219=VECTOR('',#8938,0.01);
#2220=VECTOR('',#8939,0.01);
#2221=VECTOR('',#8944,0.01);
#2222=VECTOR('',#8951,0.01);
#2223=VECTOR('',#8954,0.01);
#2224=VECTOR('',#8963,0.00118970100010167);
#2225=VECTOR('',#8966,0.00118970100010167);
#2226=VECTOR('',#8969,0.00118970099999992);
#2227=VECTOR('',#8976,0.00118970000000007);
#2228=VECTOR('',#8981,0.01);
#2229=VECTOR('',#8982,0.01);
#2230=VECTOR('',#8985,0.01);
#2231=VECTOR('',#8990,0.00118970100000004);
#2232=VECTOR('',#8995,0.01);
#2233=VECTOR('',#8996,0.01);
#2234=VECTOR('',#8997,0.01);
#2235=VECTOR('',#9000,0.01);
#2236=VECTOR('',#9005,0.01);
#2237=VECTOR('',#9006,0.01);
#2238=VECTOR('',#9009,0.01);
#2239=VECTOR('',#9018,0.00118970000000007);
#2240=VECTOR('',#9023,0.01);
#2241=VECTOR('',#9024,0.01);
#2242=VECTOR('',#9027,0.01);
#2243=VECTOR('',#9032,0.00118970100000004);
#2244=VECTOR('',#9037,0.01);
#2245=VECTOR('',#9038,0.01);
#2246=VECTOR('',#9039,0.01);
#2247=VECTOR('',#9042,0.01);
#2248=VECTOR('',#9047,0.01);
#2249=VECTOR('',#9048,0.01);
#2250=VECTOR('',#9051,0.01);
#2251=VECTOR('',#9078,0.0249999998982604);
#2252=VECTOR('',#9091,0.025);
#2253=VECTOR('',#9104,0.025);
#2254=VECTOR('',#9117,0.035);
#2255=VECTOR('',#9128,0.0249999998982604);
#2256=VECTOR('',#9141,0.025);
#2257=VECTOR('',#9164,0.028);
#2258=VECTOR('',#9173,0.01);
#2259=VECTOR('',#9174,0.01);
#2260=VECTOR('',#9191,0.025);
#2261=VECTOR('',#9196,0.0049999999999998);
#2262=VECTOR('',#9201,0.005);
#2263=VECTOR('',#9206,0.0049999999999998);
#2264=VECTOR('',#9211,0.005);
#2265=VECTOR('',#9214,0.01);
#2266=VECTOR('',#9215,0.01);
#2267=VECTOR('',#9216,0.01);
#2268=VECTOR('',#9221,0.01);
#2269=VECTOR('',#9224,0.01);
#2270=VECTOR('',#9229,0.01);
#2271=VECTOR('',#9240,0.025);
#2272=VECTOR('',#9253,0.174999999);
#2273=VECTOR('',#9260,0.025);
#2274=VECTOR('',#9273,0.174999999);
#2275=VECTOR('',#9280,0.025);
#2276=CIRCLE('',#6410,0.00749999975240882);
#2277=CIRCLE('',#6411,0.00749999975240882);
#2278=CIRCLE('',#6413,0.042);
#2279=CIRCLE('',#6414,0.042);
#2280=CIRCLE('',#6415,0.042);
#2281=CIRCLE('',#6417,0.05);
#2282=CIRCLE('',#6419,0.05);
#2283=CIRCLE('',#6420,0.05);
#2284=CIRCLE('',#6422,0.05);
#2285=CIRCLE('',#6424,0.05);
#2286=CIRCLE('',#6426,0.04);
#2287=CIRCLE('',#6428,0.04);
#2288=CIRCLE('',#6430,0.04);
#2289=CIRCLE('',#6432,0.04);
#2290=CIRCLE('',#6434,0.0025);
#2291=CIRCLE('',#6435,0.0025);
#2292=CIRCLE('',#6436,0.0025);
#2293=CIRCLE('',#6437,0.0025);
#2294=CIRCLE('',#6438,0.0025);
#2295=CIRCLE('',#6439,0.0025);
#2296=CIRCLE('',#6440,0.028);
#2297=CIRCLE('',#6442,0.0025);
#2298=CIRCLE('',#6443,0.0025);
#2299=CIRCLE('',#6444,0.0025);
#2300=CIRCLE('',#6445,0.0025);
#2301=CIRCLE('',#6446,0.0025);
#2302=CIRCLE('',#6447,0.0025);
#2303=CIRCLE('',#6448,0.028);
#2304=CIRCLE('',#6450,0.028);
#2305=CIRCLE('',#6458,0.028);
#2306=CIRCLE('',#6463,0.0248999997701383);
#2307=CIRCLE('',#6464,0.00110000131901909);
#2308=CIRCLE('',#6465,0.0260000002475909);
#2309=CIRCLE('',#6466,0.00110000131901909);
#2310=CIRCLE('',#6468,0.0248999997701383);
#2311=CIRCLE('',#6469,0.0260000002475909);
#2312=CIRCLE('',#6471,0.026);
#2313=CIRCLE('',#6472,0.026);
#2314=CIRCLE('',#6474,0.02045);
#2315=CIRCLE('',#6476,0.00110000131901911);
#2316=CIRCLE('',#6477,0.0248999997701383);
#2317=CIRCLE('',#6478,0.0011000013190191);
#2318=CIRCLE('',#6480,0.02045);
#2319=CIRCLE('',#6481,0.02045);
#2320=CIRCLE('',#6483,0.0248999997701383);
#2321=CIRCLE('',#6485,0.02045);
#2322=CIRCLE('',#6487,0.00555000054498457);
#2323=CIRCLE('',#6488,0.0130499999271107);
#2324=CIRCLE('',#6489,0.0130499999271107);
#2325=CIRCLE('',#6491,0.02045);
#2326=CIRCLE('',#6492,0.02045);
#2327=CIRCLE('',#6494,0.01305);
#2328=CIRCLE('',#6496,0.01305);
#2329=CIRCLE('',#6497,0.00555000054498457);
#2330=CIRCLE('',#6498,0.01305);
#2331=CIRCLE('',#6500,0.00860000022986177);
#2332=CIRCLE('',#6501,0.00860000022986177);
#2333=CIRCLE('',#6503,0.01305);
#2334=CIRCLE('',#6505,0.00110000131901912);
#2335=CIRCLE('',#6506,0.00749999975240907);
#2336=CIRCLE('',#6507,0.00110000131901912);
#2337=CIRCLE('',#6509,0.00749999975240873);
#2338=CIRCLE('',#6511,0.00860000022986177);
#2339=CIRCLE('',#6512,0.00860000022986177);
#2340=CIRCLE('',#6514,0.0075);
#2341=CIRCLE('',#6515,0.00749999975240873);
#2342=CIRCLE('',#6517,0.00110000131901912);
#2343=CIRCLE('',#6518,0.00110000131901912);
#2344=CIRCLE('',#6522,0.0248999997701383);
#2345=CIRCLE('',#6523,0.00110000131901909);
#2346=CIRCLE('',#6524,0.0260000002475909);
#2347=CIRCLE('',#6525,0.00110000131901909);
#2348=CIRCLE('',#6527,0.0248999997701383);
#2349=CIRCLE('',#6528,0.0260000002475909);
#2350=CIRCLE('',#6530,0.026);
#2351=CIRCLE('',#6531,0.026);
#2352=CIRCLE('',#6533,0.02045);
#2353=CIRCLE('',#6535,0.00110000131901911);
#2354=CIRCLE('',#6536,0.0248999997701383);
#2355=CIRCLE('',#6537,0.0011000013190191);
#2356=CIRCLE('',#6539,0.02045);
#2357=CIRCLE('',#6540,0.02045);
#2358=CIRCLE('',#6542,0.0248999997701383);
#2359=CIRCLE('',#6544,0.02045);
#2360=CIRCLE('',#6546,0.00555000054498457);
#2361=CIRCLE('',#6547,0.0130499999271107);
#2362=CIRCLE('',#6548,0.0130499999271107);
#2363=CIRCLE('',#6550,0.02045);
#2364=CIRCLE('',#6551,0.02045);
#2365=CIRCLE('',#6553,0.01305);
#2366=CIRCLE('',#6555,0.01305);
#2367=CIRCLE('',#6556,0.00555000054498457);
#2368=CIRCLE('',#6557,0.01305);
#2369=CIRCLE('',#6559,0.00860000022986177);
#2370=CIRCLE('',#6560,0.00860000022986177);
#2371=CIRCLE('',#6562,0.01305);
#2372=CIRCLE('',#6564,0.00110000131901912);
#2373=CIRCLE('',#6565,0.00749999975240907);
#2374=CIRCLE('',#6566,0.00110000131901912);
#2375=CIRCLE('',#6568,0.00749999975240873);
#2376=CIRCLE('',#6570,0.00860000022986177);
#2377=CIRCLE('',#6571,0.00860000022986177);
#2378=CIRCLE('',#6573,0.0075);
#2379=CIRCLE('',#6574,0.00749999975240873);
#2380=CIRCLE('',#6576,0.00110000131901912);
#2381=CIRCLE('',#6577,0.00110000131901912);
#2382=CIRCLE('',#6581,0.042);
#2383=CIRCLE('',#6582,0.042);
#2384=CIRCLE('',#6583,0.042);
#2385=CIRCLE('',#6585,0.05);
#2386=CIRCLE('',#6587,0.05);
#2387=CIRCLE('',#6588,0.05);
#2388=CIRCLE('',#6590,0.05);
#2389=CIRCLE('',#6592,0.05);
#2390=CIRCLE('',#6594,0.04);
#2391=CIRCLE('',#6596,0.04);
#2392=CIRCLE('',#6598,0.04);
#2393=CIRCLE('',#6600,0.04);
#2394=CIRCLE('',#6602,0.0025);
#2395=CIRCLE('',#6603,0.0025);
#2396=CIRCLE('',#6604,0.0025);
#2397=CIRCLE('',#6605,0.0025);
#2398=CIRCLE('',#6606,0.0025);
#2399=CIRCLE('',#6607,0.0025);
#2400=CIRCLE('',#6608,0.028);
#2401=CIRCLE('',#6610,0.0025);
#2402=CIRCLE('',#6611,0.0025);
#2403=CIRCLE('',#6612,0.0025);
#2404=CIRCLE('',#6613,0.0025);
#2405=CIRCLE('',#6614,0.0025);
#2406=CIRCLE('',#6615,0.0025);
#2407=CIRCLE('',#6616,0.028);
#2408=CIRCLE('',#6618,0.028);
#2409=CIRCLE('',#6626,0.028);
#2410=CIRCLE('',#6628,0.025);
#2411=CIRCLE('',#6630,0.025);
#2412=CIRCLE('',#6634,0.042);
#2413=CIRCLE('',#6635,0.042);
#2414=CIRCLE('',#6638,0.05);
#2415=CIRCLE('',#6640,0.05);
#2416=CIRCLE('',#6643,0.0419999999999999);
#2417=CIRCLE('',#6644,0.0420000000000001);
#2418=CIRCLE('',#6651,0.05);
#2419=CIRCLE('',#6653,0.0500000000000661);
#2420=CIRCLE('',#6659,0.005);
#2421=CIRCLE('',#6660,0.005);
#2422=CIRCLE('',#6662,0.005);
#2423=CIRCLE('',#6663,0.025);
#2424=CIRCLE('',#6664,0.005);
#2425=CIRCLE('',#6665,0.005);
#2426=CIRCLE('',#6667,0.005);
#2427=CIRCLE('',#6668,0.025);
#2428=CIRCLE('',#6669,0.005);
#2429=CIRCLE('',#6670,0.005);
#2430=CIRCLE('',#6681,0.0248999997701383);
#2431=CIRCLE('',#6682,0.00110000131901909);
#2432=CIRCLE('',#6683,0.0260000002475909);
#2433=CIRCLE('',#6684,0.00110000131901909);
#2434=CIRCLE('',#6686,0.0248999997701383);
#2435=CIRCLE('',#6687,0.0260000002475909);
#2436=CIRCLE('',#6689,0.026);
#2437=CIRCLE('',#6690,0.026);
#2438=CIRCLE('',#6692,0.02045);
#2439=CIRCLE('',#6694,0.00110000131901911);
#2440=CIRCLE('',#6695,0.0248999997701383);
#2441=CIRCLE('',#6696,0.0011000013190191);
#2442=CIRCLE('',#6698,0.02045);
#2443=CIRCLE('',#6699,0.02045);
#2444=CIRCLE('',#6701,0.0248999997701383);
#2445=CIRCLE('',#6703,0.02045);
#2446=CIRCLE('',#6705,0.00555000054498457);
#2447=CIRCLE('',#6706,0.0130499999271107);
#2448=CIRCLE('',#6707,0.0130499999271107);
#2449=CIRCLE('',#6709,0.02045);
#2450=CIRCLE('',#6710,0.02045);
#2451=CIRCLE('',#6712,0.01305);
#2452=CIRCLE('',#6714,0.01305);
#2453=CIRCLE('',#6715,0.00555000054498457);
#2454=CIRCLE('',#6716,0.01305);
#2455=CIRCLE('',#6718,0.00860000022986177);
#2456=CIRCLE('',#6719,0.00860000022986177);
#2457=CIRCLE('',#6721,0.01305);
#2458=CIRCLE('',#6723,0.00110000131901912);
#2459=CIRCLE('',#6724,0.00749999975240907);
#2460=CIRCLE('',#6725,0.00110000131901912);
#2461=CIRCLE('',#6727,0.00749999975240873);
#2462=CIRCLE('',#6729,0.00860000022986177);
#2463=CIRCLE('',#6730,0.00860000022986177);
#2464=CIRCLE('',#6732,0.0075);
#2465=CIRCLE('',#6733,0.00749999975240873);
#2466=CIRCLE('',#6735,0.00110000131901912);
#2467=CIRCLE('',#6736,0.00110000131901912);
#2468=CIRCLE('',#6740,0.028);
#2469=CIRCLE('',#6741,0.028);
#2470=CIRCLE('',#6743,0.025);
#2471=CIRCLE('',#6745,0.299);
#2472=CIRCLE('',#6746,0.05);
#2473=CIRCLE('',#6747,0.005);
#2474=CIRCLE('',#6748,0.0049999999999998);
#2475=CIRCLE('',#6749,0.005);
#2476=CIRCLE('',#6750,0.0049999999999998);
#2477=CIRCLE('',#6752,0.025);
#2478=CIRCLE('',#6754,0.0049999999999998);
#2479=CIRCLE('',#6756,0.005);
#2480=CIRCLE('',#6758,0.0049999999999998);
#2481=CIRCLE('',#6760,0.005);
#2482=CIRCLE('',#6764,0.05);
#2483=CIRCLE('',#6766,0.299);
#2484=CIRCLE('',#6770,0.0248999997701383);
#2485=CIRCLE('',#6771,0.00110000131901909);
#2486=CIRCLE('',#6772,0.0260000002475909);
#2487=CIRCLE('',#6773,0.00110000131901909);
#2488=CIRCLE('',#6775,0.0248999997701383);
#2489=CIRCLE('',#6776,0.0260000002475909);
#2490=CIRCLE('',#6778,0.026);
#2491=CIRCLE('',#6779,0.026);
#2492=CIRCLE('',#6781,0.02045);
#2493=CIRCLE('',#6783,0.00110000131901911);
#2494=CIRCLE('',#6784,0.0248999997701383);
#2495=CIRCLE('',#6785,0.0011000013190191);
#2496=CIRCLE('',#6787,0.02045);
#2497=CIRCLE('',#6788,0.02045);
#2498=CIRCLE('',#6790,0.0248999997701383);
#2499=CIRCLE('',#6792,0.02045);
#2500=CIRCLE('',#6794,0.00555000054498457);
#2501=CIRCLE('',#6795,0.0130499999271107);
#2502=CIRCLE('',#6796,0.0130499999271107);
#2503=CIRCLE('',#6798,0.02045);
#2504=CIRCLE('',#6799,0.02045);
#2505=CIRCLE('',#6801,0.01305);
#2506=CIRCLE('',#6803,0.01305);
#2507=CIRCLE('',#6804,0.00555000054498457);
#2508=CIRCLE('',#6805,0.01305);
#2509=CIRCLE('',#6807,0.00860000022986177);
#2510=CIRCLE('',#6808,0.00860000022986177);
#2511=CIRCLE('',#6810,0.01305);
#2512=CIRCLE('',#6812,0.00110000131901912);
#2513=CIRCLE('',#6813,0.00749999975240907);
#2514=CIRCLE('',#6814,0.00110000131901912);
#2515=CIRCLE('',#6816,0.00749999975240873);
#2516=CIRCLE('',#6818,0.00860000022986177);
#2517=CIRCLE('',#6819,0.00860000022986177);
#2518=CIRCLE('',#6821,0.0075);
#2519=CIRCLE('',#6822,0.00749999975240873);
#2520=CIRCLE('',#6824,0.00110000131901912);
#2521=CIRCLE('',#6825,0.00110000131901912);
#2522=CIRCLE('',#6830,0.00799999973819874);
#2523=CIRCLE('',#6831,0.00799999973819874);
#2524=CIRCLE('',#6834,0.00999999988959839);
#2525=CIRCLE('',#6836,0.00999999988959839);
#2526=CIRCLE('',#6840,0.00799999961340774);
#2527=CIRCLE('',#6841,0.00799999961340774);
#2528=CIRCLE('',#6842,0.00799999961340774);
#2529=CIRCLE('',#6843,0.00799999961340774);
#2530=CIRCLE('',#6844,0.00799999961340774);
#2531=CIRCLE('',#6845,0.00799999961340774);
#2532=CIRCLE('',#6846,0.00799999961340774);
#2533=CIRCLE('',#6847,0.00799999961340774);
#2534=CIRCLE('',#6862,0.00799999959059736);
#2535=CIRCLE('',#6863,0.00799999959059736);
#2536=CIRCLE('',#6866,0.0099999996557502);
#2537=CIRCLE('',#6868,0.0099999996557502);
#2538=CIRCLE('',#6872,0.00799999974118007);
#2539=CIRCLE('',#6873,0.00799999974118007);
#2540=CIRCLE('',#6874,0.00799999974118007);
#2541=CIRCLE('',#6875,0.00799999974118007);
#2542=CIRCLE('',#6876,0.00799999974118007);
#2543=CIRCLE('',#6877,0.00799999974118007);
#2544=CIRCLE('',#6878,0.00799999974118007);
#2545=CIRCLE('',#6879,0.00799999974118007);
#2546=CIRCLE('',#6894,0.0079999999576051);
#2547=CIRCLE('',#6895,0.0079999999576051);
#2548=CIRCLE('',#6896,0.0079999999576051);
#2549=CIRCLE('',#6897,0.0079999999576051);
#2550=CIRCLE('',#6898,0.0079999999576051);
#2551=CIRCLE('',#6899,0.0079999999576051);
#2552=CIRCLE('',#6900,0.0079999999576051);
#2553=CIRCLE('',#6901,0.0079999999576051);
#2554=CIRCLE('',#6916,0.00799999974106502);
#2555=CIRCLE('',#6917,0.00799999974106502);
#2556=CIRCLE('',#6920,0.00999999987547767);
#2557=CIRCLE('',#6922,0.00999999987547767);
#2558=CIRCLE('',#6926,0.00749999975240907);
#2559=CIRCLE('',#6927,0.0075);
#2560=CIRCLE('',#6928,0.0075);
#2561=CIRCLE('',#6929,0.00749999975240907);
#2562=CIRCLE('',#6931,0.00749999975240883);
#2563=CIRCLE('',#6932,0.0075);
#2564=CIRCLE('',#6933,0.0075);
#2565=CIRCLE('',#6935,0.00749999975240907);
#2566=CIRCLE('',#6936,0.00749999975240883);
#2567=CIRCLE('',#6937,0.00749999975240907);
#2568=CIRCLE('',#6939,0.0075);
#2569=CIRCLE('',#6940,0.00749999975240883);
#2570=CIRCLE('',#6942,0.00749999975240883);
#2571=CIRCLE('',#6943,0.00749999975240907);
#2572=CIRCLE('',#6945,0.015);
#2573=CIRCLE('',#6948,0.015);
#2574=CIRCLE('',#6963,0.01);
#2575=CIRCLE('',#6964,0.01);
#2576=CIRCLE('',#6966,0.00499999999997558);
#2577=CIRCLE('',#6967,0.00499999999997557);
#2578=CIRCLE('',#6968,0.00500000000000013);
#2579=CIRCLE('',#6969,0.005);
#2580=CIRCLE('',#6970,0.005);
#2581=CIRCLE('',#6971,0.00500000000000013);
#2582=CIRCLE('',#6972,0.00499999999997558);
#2583=CIRCLE('',#6973,0.00499999999997557);
#2584=CIRCLE('',#6975,0.00499999999997558);
#2585=CIRCLE('',#6976,0.00499999999997557);
#2586=CIRCLE('',#6977,0.00500000000000013);
#2587=CIRCLE('',#6978,0.005);
#2588=CIRCLE('',#6979,0.005);
#2589=CIRCLE('',#6980,0.00500000000000013);
#2590=CIRCLE('',#6981,0.00499999999997558);
#2591=CIRCLE('',#6982,0.00499999999997557);
#2592=CIRCLE('',#7001,0.01);
#2593=CIRCLE('',#7002,0.005);
#2594=CIRCLE('',#7003,0.005);
#2595=CIRCLE('',#7004,0.00500000000000013);
#2596=CIRCLE('',#7005,0.005);
#2597=CIRCLE('',#7006,0.005);
#2598=CIRCLE('',#7007,0.00500000000000013);
#2599=CIRCLE('',#7008,0.005);
#2600=CIRCLE('',#7009,0.005);
#2601=CIRCLE('',#7011,0.01);
#2602=CIRCLE('',#7012,0.005);
#2603=CIRCLE('',#7013,0.005);
#2604=CIRCLE('',#7014,0.00500000000000013);
#2605=CIRCLE('',#7015,0.005);
#2606=CIRCLE('',#7016,0.005);
#2607=CIRCLE('',#7017,0.00500000000000013);
#2608=CIRCLE('',#7018,0.005);
#2609=CIRCLE('',#7019,0.005);
#2610=CIRCLE('',#7032,0.003);
#2611=CIRCLE('',#7033,0.003);
#2612=CIRCLE('',#7036,0.0125);
#2613=CIRCLE('',#7038,0.0125);
#2614=CIRCLE('',#7040,0.003);
#2615=CIRCLE('',#7042,0.003);
#2616=CIRCLE('',#7047,0.00118970000000007);
#2617=CIRCLE('',#7048,0.00118970000000007);
#2618=CIRCLE('',#7050,0.007216878);
#2619=CIRCLE('',#7051,0.00118970100000004);
#2620=CIRCLE('',#7053,0.00118970100000004);
#2621=CIRCLE('',#7056,0.007216878);
#2622=CIRCLE('',#7069,0.00118970000000007);
#2623=CIRCLE('',#7070,0.00118970000000007);
#2624=CIRCLE('',#7072,0.007216878);
#2625=CIRCLE('',#7073,0.00118970100000004);
#2626=CIRCLE('',#7075,0.00118970100000004);
#2627=CIRCLE('',#7078,0.007216878);
#2628=CIRCLE('',#7084,0.00118970099999992);
#2629=CIRCLE('',#7085,0.00118970099999992);
#2630=CIRCLE('',#7087,0.00118970100010167);
#2631=CIRCLE('',#7088,0.00118970100010167);
#2632=CIRCLE('',#7095,0.00118970099999992);
#2633=CIRCLE('',#7098,0.00118970099999992);
#2634=CIRCLE('',#7101,0.00118970100010167);
#2635=CIRCLE('',#7102,0.00118970100010167);
#2636=CIRCLE('',#7109,0.00118970000000007);
#2637=CIRCLE('',#7110,0.00118970000000007);
#2638=CIRCLE('',#7112,0.007216878);
#2639=CIRCLE('',#7113,0.00118970100000004);
#2640=CIRCLE('',#7115,0.00118970100000004);
#2641=CIRCLE('',#7118,0.007216878);
#2642=CIRCLE('',#7124,0.00118970000000007);
#2643=CIRCLE('',#7125,0.00118970000000007);
#2644=CIRCLE('',#7127,0.007216878);
#2645=CIRCLE('',#7128,0.00118970100000004);
#2646=CIRCLE('',#7130,0.00118970100000004);
#2647=CIRCLE('',#7133,0.007216878);
#2648=CIRCLE('',#7154,0.025);
#2649=CIRCLE('',#7155,0.025);
#2650=CIRCLE('',#7160,0.025);
#2651=CIRCLE('',#7161,0.025);
#2652=CIRCLE('',#7163,0.035);
#2653=CIRCLE('',#7165,0.035);
#2654=CIRCLE('',#7177,0.025);
#2655=CIRCLE('',#7178,0.025);
#2656=CIRCLE('',#7188,0.028);
#2657=CIRCLE('',#7189,0.028);
#2658=CIRCLE('',#7191,0.025);
#2659=CIRCLE('',#7193,0.299);
#2660=CIRCLE('',#7194,0.05);
#2661=CIRCLE('',#7195,0.005);
#2662=CIRCLE('',#7196,0.0049999999999998);
#2663=CIRCLE('',#7197,0.005);
#2664=CIRCLE('',#7198,0.0049999999999998);
#2665=CIRCLE('',#7200,0.025);
#2666=CIRCLE('',#7202,0.0049999999999998);
#2667=CIRCLE('',#7204,0.005);
#2668=CIRCLE('',#7206,0.0049999999999998);
#2669=CIRCLE('',#7208,0.005);
#2670=CIRCLE('',#7211,0.299);
#2671=CIRCLE('',#7213,0.05);
#2672=CIRCLE('',#7219,0.025);
#2673=CIRCLE('',#7220,0.025);
#2674=CIRCLE('',#7222,0.174999999);
#2675=CIRCLE('',#7224,0.174999999);
#2676=CIRCLE('',#7228,0.025);
#2677=CIRCLE('',#7229,0.025);
#2678=CIRCLE('',#7231,0.174999999);
#2679=CIRCLE('',#7233,0.174999999);
#2680=CIRCLE('',#7237,0.025);
#2681=CIRCLE('',#7238,0.025);
#2682=VERTEX_POINT('',#9328);
#2683=VERTEX_POINT('',#9330);
#2684=VERTEX_POINT('',#9334);
#2685=VERTEX_POINT('',#9336);
#2686=VERTEX_POINT('',#9338);
#2687=VERTEX_POINT('',#9342);
#2688=VERTEX_POINT('',#9346);
#2689=VERTEX_POINT('',#9347);
#2690=VERTEX_POINT('',#9352);
#2691=VERTEX_POINT('',#9356);
#2692=VERTEX_POINT('',#9360);
#2693=VERTEX_POINT('',#9363);
#2694=VERTEX_POINT('',#9366);
#2695=VERTEX_POINT('',#9370);
#2696=VERTEX_POINT('',#9374);
#2697=VERTEX_POINT('',#9376);
#2698=VERTEX_POINT('',#9378);
#2699=VERTEX_POINT('',#9380);
#2700=VERTEX_POINT('',#9382);
#2701=VERTEX_POINT('',#9384);
#2702=VERTEX_POINT('',#9386);
#2703=VERTEX_POINT('',#9389);
#2704=VERTEX_POINT('',#9391);
#2705=VERTEX_POINT('',#9393);
#2706=VERTEX_POINT('',#9395);
#2707=VERTEX_POINT('',#9397);
#2708=VERTEX_POINT('',#9399);
#2709=VERTEX_POINT('',#9401);
#2710=VERTEX_POINT('',#9404);
#2711=VERTEX_POINT('',#9420);
#2712=VERTEX_POINT('',#9427);
#2713=VERTEX_POINT('',#9428);
#2714=VERTEX_POINT('',#9430);
#2715=VERTEX_POINT('',#9432);
#2716=VERTEX_POINT('',#9439);
#2717=VERTEX_POINT('',#9440);
#2718=VERTEX_POINT('',#9445);
#2719=VERTEX_POINT('',#9448);
#2720=VERTEX_POINT('',#9450);
#2721=VERTEX_POINT('',#9454);
#2722=VERTEX_POINT('',#9456);
#2723=VERTEX_POINT('',#9462);
#2724=VERTEX_POINT('',#9465);
#2725=VERTEX_POINT('',#9467);
#2726=VERTEX_POINT('',#9471);
#2727=VERTEX_POINT('',#9472);
#2728=VERTEX_POINT('',#9477);
#2729=VERTEX_POINT('',#9481);
#2730=VERTEX_POINT('',#9482);
#2731=VERTEX_POINT('',#9487);
#2732=VERTEX_POINT('',#9488);
#2733=VERTEX_POINT('',#9492);
#2734=VERTEX_POINT('',#9496);
#2735=VERTEX_POINT('',#9498);
#2736=VERTEX_POINT('',#9504);
#2737=VERTEX_POINT('',#9505);
#2738=VERTEX_POINT('',#9509);
#2739=VERTEX_POINT('',#9511);
#2740=VERTEX_POINT('',#9520);
#2741=VERTEX_POINT('',#9521);
#2742=VERTEX_POINT('',#9523);
#2743=VERTEX_POINT('',#9525);
#2744=VERTEX_POINT('',#9532);
#2745=VERTEX_POINT('',#9533);
#2746=VERTEX_POINT('',#9538);
#2747=VERTEX_POINT('',#9541);
#2748=VERTEX_POINT('',#9543);
#2749=VERTEX_POINT('',#9547);
#2750=VERTEX_POINT('',#9549);
#2751=VERTEX_POINT('',#9555);
#2752=VERTEX_POINT('',#9558);
#2753=VERTEX_POINT('',#9560);
#2754=VERTEX_POINT('',#9564);
#2755=VERTEX_POINT('',#9565);
#2756=VERTEX_POINT('',#9570);
#2757=VERTEX_POINT('',#9574);
#2758=VERTEX_POINT('',#9575);
#2759=VERTEX_POINT('',#9580);
#2760=VERTEX_POINT('',#9581);
#2761=VERTEX_POINT('',#9585);
#2762=VERTEX_POINT('',#9589);
#2763=VERTEX_POINT('',#9591);
#2764=VERTEX_POINT('',#9597);
#2765=VERTEX_POINT('',#9598);
#2766=VERTEX_POINT('',#9602);
#2767=VERTEX_POINT('',#9604);
#2768=VERTEX_POINT('',#9613);
#2769=VERTEX_POINT('',#9615);
#2770=VERTEX_POINT('',#9617);
#2771=VERTEX_POINT('',#9621);
#2772=VERTEX_POINT('',#9625);
#2773=VERTEX_POINT('',#9626);
#2774=VERTEX_POINT('',#9631);
#2775=VERTEX_POINT('',#9635);
#2776=VERTEX_POINT('',#9639);
#2777=VERTEX_POINT('',#9642);
#2778=VERTEX_POINT('',#9645);
#2779=VERTEX_POINT('',#9649);
#2780=VERTEX_POINT('',#9653);
#2781=VERTEX_POINT('',#9655);
#2782=VERTEX_POINT('',#9657);
#2783=VERTEX_POINT('',#9659);
#2784=VERTEX_POINT('',#9661);
#2785=VERTEX_POINT('',#9663);
#2786=VERTEX_POINT('',#9665);
#2787=VERTEX_POINT('',#9668);
#2788=VERTEX_POINT('',#9670);
#2789=VERTEX_POINT('',#9672);
#2790=VERTEX_POINT('',#9674);
#2791=VERTEX_POINT('',#9676);
#2792=VERTEX_POINT('',#9678);
#2793=VERTEX_POINT('',#9680);
#2794=VERTEX_POINT('',#9683);
#2795=VERTEX_POINT('',#9699);
#2796=VERTEX_POINT('',#9703);
#2797=VERTEX_POINT('',#9706);
#2798=VERTEX_POINT('',#9712);
#2799=VERTEX_POINT('',#9713);
#2800=VERTEX_POINT('',#9715);
#2801=VERTEX_POINT('',#9717);
#2802=VERTEX_POINT('',#9721);
#2803=VERTEX_POINT('',#9723);
#2804=VERTEX_POINT('',#9727);
#2805=VERTEX_POINT('',#9729);
#2806=VERTEX_POINT('',#9733);
#2807=VERTEX_POINT('',#9734);
#2808=VERTEX_POINT('',#9739);
#2809=VERTEX_POINT('',#9743);
#2810=VERTEX_POINT('',#9744);
#2811=VERTEX_POINT('',#9749);
#2812=VERTEX_POINT('',#9759);
#2813=VERTEX_POINT('',#9765);
#2814=VERTEX_POINT('',#9777);
#2815=VERTEX_POINT('',#9779);
#2816=VERTEX_POINT('',#9783);
#2817=VERTEX_POINT('',#9784);
#2818=VERTEX_POINT('',#9786);
#2819=VERTEX_POINT('',#9788);
#2820=VERTEX_POINT('',#9791);
#2821=VERTEX_POINT('',#9793);
#2822=VERTEX_POINT('',#9795);
#2823=VERTEX_POINT('',#9797);
#2824=VERTEX_POINT('',#9800);
#2825=VERTEX_POINT('',#9801);
#2826=VERTEX_POINT('',#9803);
#2827=VERTEX_POINT('',#9805);
#2828=VERTEX_POINT('',#9808);
#2829=VERTEX_POINT('',#9810);
#2830=VERTEX_POINT('',#9812);
#2831=VERTEX_POINT('',#9814);
#2832=VERTEX_POINT('',#9834);
#2833=VERTEX_POINT('',#9835);
#2834=VERTEX_POINT('',#9837);
#2835=VERTEX_POINT('',#9839);
#2836=VERTEX_POINT('',#9846);
#2837=VERTEX_POINT('',#9847);
#2838=VERTEX_POINT('',#9852);
#2839=VERTEX_POINT('',#9855);
#2840=VERTEX_POINT('',#9857);
#2841=VERTEX_POINT('',#9861);
#2842=VERTEX_POINT('',#9863);
#2843=VERTEX_POINT('',#9869);
#2844=VERTEX_POINT('',#9872);
#2845=VERTEX_POINT('',#9874);
#2846=VERTEX_POINT('',#9878);
#2847=VERTEX_POINT('',#9879);
#2848=VERTEX_POINT('',#9884);
#2849=VERTEX_POINT('',#9888);
#2850=VERTEX_POINT('',#9889);
#2851=VERTEX_POINT('',#9894);
#2852=VERTEX_POINT('',#9895);
#2853=VERTEX_POINT('',#9899);
#2854=VERTEX_POINT('',#9903);
#2855=VERTEX_POINT('',#9905);
#2856=VERTEX_POINT('',#9911);
#2857=VERTEX_POINT('',#9912);
#2858=VERTEX_POINT('',#9916);
#2859=VERTEX_POINT('',#9918);
#2860=VERTEX_POINT('',#9927);
#2861=VERTEX_POINT('',#9929);
#2862=VERTEX_POINT('',#9933);
#2863=VERTEX_POINT('',#9936);
#2864=VERTEX_POINT('',#9937);
#2865=VERTEX_POINT('',#9939);
#2866=VERTEX_POINT('',#9941);
#2867=VERTEX_POINT('',#9944);
#2868=VERTEX_POINT('',#9946);
#2869=VERTEX_POINT('',#9948);
#2870=VERTEX_POINT('',#9950);
#2871=VERTEX_POINT('',#9953);
#2872=VERTEX_POINT('',#9957);
#2873=VERTEX_POINT('',#9961);
#2874=VERTEX_POINT('',#9965);
#2875=VERTEX_POINT('',#9969);
#2876=VERTEX_POINT('',#9973);
#2877=VERTEX_POINT('',#9975);
#2878=VERTEX_POINT('',#9979);
#2879=VERTEX_POINT('',#9983);
#2880=VERTEX_POINT('',#9991);
#2881=VERTEX_POINT('',#9992);
#2882=VERTEX_POINT('',#9994);
#2883=VERTEX_POINT('',#9996);
#2884=VERTEX_POINT('',#10003);
#2885=VERTEX_POINT('',#10004);
#2886=VERTEX_POINT('',#10009);
#2887=VERTEX_POINT('',#10012);
#2888=VERTEX_POINT('',#10014);
#2889=VERTEX_POINT('',#10018);
#2890=VERTEX_POINT('',#10020);
#2891=VERTEX_POINT('',#10026);
#2892=VERTEX_POINT('',#10029);
#2893=VERTEX_POINT('',#10031);
#2894=VERTEX_POINT('',#10035);
#2895=VERTEX_POINT('',#10036);
#2896=VERTEX_POINT('',#10041);
#2897=VERTEX_POINT('',#10045);
#2898=VERTEX_POINT('',#10046);
#2899=VERTEX_POINT('',#10051);
#2900=VERTEX_POINT('',#10052);
#2901=VERTEX_POINT('',#10056);
#2902=VERTEX_POINT('',#10060);
#2903=VERTEX_POINT('',#10062);
#2904=VERTEX_POINT('',#10068);
#2905=VERTEX_POINT('',#10069);
#2906=VERTEX_POINT('',#10073);
#2907=VERTEX_POINT('',#10075);
#2908=VERTEX_POINT('',#10085);
#2909=VERTEX_POINT('',#10087);
#2910=VERTEX_POINT('',#10092);
#2911=VERTEX_POINT('',#10095);
#2912=VERTEX_POINT('',#10101);
#2913=VERTEX_POINT('',#10102);
#2914=VERTEX_POINT('',#10104);
#2915=VERTEX_POINT('',#10106);
#2916=VERTEX_POINT('',#10108);
#2917=VERTEX_POINT('',#10110);
#2918=VERTEX_POINT('',#10113);
#2919=VERTEX_POINT('',#10115);
#2920=VERTEX_POINT('',#10122);
#2921=VERTEX_POINT('',#10126);
#2922=VERTEX_POINT('',#10132);
#2923=VERTEX_POINT('',#10136);
#2924=VERTEX_POINT('',#10140);
#2925=VERTEX_POINT('',#10142);
#2926=VERTEX_POINT('',#10146);
#2927=VERTEX_POINT('',#10150);
#2928=VERTEX_POINT('',#10158);
#2929=VERTEX_POINT('',#10160);
#2930=VERTEX_POINT('',#10165);
#2931=VERTEX_POINT('',#10168);
#2932=VERTEX_POINT('',#10174);
#2933=VERTEX_POINT('',#10175);
#2934=VERTEX_POINT('',#10177);
#2935=VERTEX_POINT('',#10179);
#2936=VERTEX_POINT('',#10181);
#2937=VERTEX_POINT('',#10183);
#2938=VERTEX_POINT('',#10186);
#2939=VERTEX_POINT('',#10188);
#2940=VERTEX_POINT('',#10195);
#2941=VERTEX_POINT('',#10199);
#2942=VERTEX_POINT('',#10205);
#2943=VERTEX_POINT('',#10209);
#2944=VERTEX_POINT('',#10213);
#2945=VERTEX_POINT('',#10215);
#2946=VERTEX_POINT('',#10219);
#2947=VERTEX_POINT('',#10223);
#2948=VERTEX_POINT('',#10231);
#2949=VERTEX_POINT('',#10232);
#2950=VERTEX_POINT('',#10234);
#2951=VERTEX_POINT('',#10236);
#2952=VERTEX_POINT('',#10238);
#2953=VERTEX_POINT('',#10240);
#2954=VERTEX_POINT('',#10243);
#2955=VERTEX_POINT('',#10245);
#2956=VERTEX_POINT('',#10252);
#2957=VERTEX_POINT('',#10256);
#2958=VERTEX_POINT('',#10262);
#2959=VERTEX_POINT('',#10266);
#2960=VERTEX_POINT('',#10270);
#2961=VERTEX_POINT('',#10272);
#2962=VERTEX_POINT('',#10276);
#2963=VERTEX_POINT('',#10280);
#2964=VERTEX_POINT('',#10288);
#2965=VERTEX_POINT('',#10290);
#2966=VERTEX_POINT('',#10295);
#2967=VERTEX_POINT('',#10298);
#2968=VERTEX_POINT('',#10304);
#2969=VERTEX_POINT('',#10305);
#2970=VERTEX_POINT('',#10307);
#2971=VERTEX_POINT('',#10309);
#2972=VERTEX_POINT('',#10314);
#2973=VERTEX_POINT('',#10316);
#2974=VERTEX_POINT('',#10318);
#2975=VERTEX_POINT('',#10322);
#2976=VERTEX_POINT('',#10323);
#2977=VERTEX_POINT('',#10325);
#2978=VERTEX_POINT('',#10330);
#2979=VERTEX_POINT('',#10332);
#2980=VERTEX_POINT('',#10336);
#2981=VERTEX_POINT('',#10338);
#2982=VERTEX_POINT('',#10342);
#2983=VERTEX_POINT('',#10347);
#2984=VERTEX_POINT('',#10366);
#2985=VERTEX_POINT('',#10368);
#2986=VERTEX_POINT('',#10372);
#2987=VERTEX_POINT('',#10373);
#2988=VERTEX_POINT('',#10375);
#2989=VERTEX_POINT('',#10377);
#2990=VERTEX_POINT('',#10380);
#2991=VERTEX_POINT('',#10382);
#2992=VERTEX_POINT('',#10384);
#2993=VERTEX_POINT('',#10386);
#2994=VERTEX_POINT('',#10388);
#2995=VERTEX_POINT('',#10390);
#2996=VERTEX_POINT('',#10392);
#2997=VERTEX_POINT('',#10394);
#2998=VERTEX_POINT('',#10397);
#2999=VERTEX_POINT('',#10398);
#3000=VERTEX_POINT('',#10400);
#3001=VERTEX_POINT('',#10402);
#3002=VERTEX_POINT('',#10404);
#3003=VERTEX_POINT('',#10406);
#3004=VERTEX_POINT('',#10408);
#3005=VERTEX_POINT('',#10410);
#3006=VERTEX_POINT('',#10413);
#3007=VERTEX_POINT('',#10415);
#3008=VERTEX_POINT('',#10417);
#3009=VERTEX_POINT('',#10419);
#3010=VERTEX_POINT('',#10421);
#3011=VERTEX_POINT('',#10423);
#3012=VERTEX_POINT('',#10425);
#3013=VERTEX_POINT('',#10427);
#3014=VERTEX_POINT('',#10446);
#3015=VERTEX_POINT('',#10447);
#3016=VERTEX_POINT('',#10449);
#3017=VERTEX_POINT('',#10451);
#3018=VERTEX_POINT('',#10461);
#3019=VERTEX_POINT('',#10463);
#3020=VERTEX_POINT('',#10465);
#3021=VERTEX_POINT('',#10469);
#3022=VERTEX_POINT('',#10473);
#3023=VERTEX_POINT('',#10477);
#3024=VERTEX_POINT('',#10483);
#3025=VERTEX_POINT('',#10484);
#3026=VERTEX_POINT('',#10490);
#3027=VERTEX_POINT('',#10492);
#3028=VERTEX_POINT('',#10494);
#3029=VERTEX_POINT('',#10496);
#3030=VERTEX_POINT('',#10498);
#3031=VERTEX_POINT('',#10500);
#3032=VERTEX_POINT('',#10502);
#3033=VERTEX_POINT('',#10504);
#3034=VERTEX_POINT('',#10506);
#3035=VERTEX_POINT('',#10510);
#3036=VERTEX_POINT('',#10512);
#3037=VERTEX_POINT('',#10514);
#3038=VERTEX_POINT('',#10516);
#3039=VERTEX_POINT('',#10518);
#3040=VERTEX_POINT('',#10520);
#3041=VERTEX_POINT('',#10522);
#3042=VERTEX_POINT('',#10524);
#3043=VERTEX_POINT('',#10526);
#3044=VERTEX_POINT('',#10549);
#3045=VERTEX_POINT('',#10551);
#3046=VERTEX_POINT('',#10556);
#3047=VERTEX_POINT('',#10559);
#3048=VERTEX_POINT('',#10563);
#3049=VERTEX_POINT('',#10566);
#3050=VERTEX_POINT('',#10573);
#3051=VERTEX_POINT('',#10575);
#3052=VERTEX_POINT('',#10579);
#3053=VERTEX_POINT('',#10580);
#3054=VERTEX_POINT('',#10582);
#3055=VERTEX_POINT('',#10584);
#3056=VERTEX_POINT('',#10587);
#3057=VERTEX_POINT('',#10590);
#3058=VERTEX_POINT('',#10594);
#3059=VERTEX_POINT('',#10596);
#3060=VERTEX_POINT('',#10600);
#3061=VERTEX_POINT('',#10604);
#3062=VERTEX_POINT('',#10612);
#3063=VERTEX_POINT('',#10613);
#3064=VERTEX_POINT('',#10615);
#3065=VERTEX_POINT('',#10617);
#3066=VERTEX_POINT('',#10621);
#3067=VERTEX_POINT('',#10623);
#3068=VERTEX_POINT('',#10627);
#3069=VERTEX_POINT('',#10631);
#3070=VERTEX_POINT('',#10639);
#3071=VERTEX_POINT('',#10641);
#3072=VERTEX_POINT('',#10645);
#3073=VERTEX_POINT('',#10646);
#3074=VERTEX_POINT('',#10648);
#3075=VERTEX_POINT('',#10650);
#3076=VERTEX_POINT('',#10653);
#3077=VERTEX_POINT('',#10656);
#3078=VERTEX_POINT('',#10660);
#3079=VERTEX_POINT('',#10662);
#3080=VERTEX_POINT('',#10666);
#3081=VERTEX_POINT('',#10670);
#3082=VERTEX_POINT('',#10678);
#3083=VERTEX_POINT('',#10680);
#3084=VERTEX_POINT('',#10684);
#3085=VERTEX_POINT('',#10685);
#3086=VERTEX_POINT('',#10687);
#3087=VERTEX_POINT('',#10689);
#3088=VERTEX_POINT('',#10691);
#3089=VERTEX_POINT('',#10693);
#3090=VERTEX_POINT('',#10696);
#3091=VERTEX_POINT('',#10698);
#3092=VERTEX_POINT('',#10701);
#3093=VERTEX_POINT('',#10702);
#3094=VERTEX_POINT('',#10704);
#3095=VERTEX_POINT('',#10706);
#3096=VERTEX_POINT('',#10708);
#3097=VERTEX_POINT('',#10711);
#3098=VERTEX_POINT('',#10715);
#3099=VERTEX_POINT('',#10719);
#3100=VERTEX_POINT('',#10723);
#3101=VERTEX_POINT('',#10727);
#3102=VERTEX_POINT('',#10728);
#3103=VERTEX_POINT('',#10730);
#3104=VERTEX_POINT('',#10732);
#3105=VERTEX_POINT('',#10734);
#3106=VERTEX_POINT('',#10741);
#3107=VERTEX_POINT('',#10746);
#3108=VERTEX_POINT('',#10752);
#3109=VERTEX_POINT('',#10754);
#3110=VERTEX_POINT('',#10765);
#3111=VERTEX_POINT('',#10767);
#3112=VERTEX_POINT('',#10771);
#3113=VERTEX_POINT('',#10772);
#3114=VERTEX_POINT('',#10774);
#3115=VERTEX_POINT('',#10776);
#3116=VERTEX_POINT('',#10779);
#3117=VERTEX_POINT('',#10782);
#3118=VERTEX_POINT('',#10786);
#3119=VERTEX_POINT('',#10788);
#3120=VERTEX_POINT('',#10792);
#3121=VERTEX_POINT('',#10796);
#3122=VERTEX_POINT('',#10804);
#3123=VERTEX_POINT('',#10806);
#3124=VERTEX_POINT('',#10810);
#3125=VERTEX_POINT('',#10811);
#3126=VERTEX_POINT('',#10813);
#3127=VERTEX_POINT('',#10815);
#3128=VERTEX_POINT('',#10818);
#3129=VERTEX_POINT('',#10821);
#3130=VERTEX_POINT('',#10825);
#3131=VERTEX_POINT('',#10827);
#3132=VERTEX_POINT('',#10831);
#3133=VERTEX_POINT('',#10835);
#3134=VERTEX_POINT('',#10850);
#3135=VERTEX_POINT('',#10851);
#3136=VERTEX_POINT('',#10855);
#3137=VERTEX_POINT('',#10857);
#3138=VERTEX_POINT('',#10863);
#3139=VERTEX_POINT('',#10865);
#3140=VERTEX_POINT('',#10872);
#3141=VERTEX_POINT('',#10874);
#3142=VERTEX_POINT('',#10878);
#3143=VERTEX_POINT('',#10881);
#3144=VERTEX_POINT('',#10887);
#3145=VERTEX_POINT('',#10888);
#3146=VERTEX_POINT('',#10892);
#3147=VERTEX_POINT('',#10894);
#3148=VERTEX_POINT('',#10900);
#3149=VERTEX_POINT('',#10902);
#3150=VERTEX_POINT('',#10914);
#3151=VERTEX_POINT('',#10916);
#3152=VERTEX_POINT('',#10920);
#3153=VERTEX_POINT('',#10923);
#3154=VERTEX_POINT('',#10924);
#3155=VERTEX_POINT('',#10926);
#3156=VERTEX_POINT('',#10928);
#3157=VERTEX_POINT('',#10931);
#3158=VERTEX_POINT('',#10933);
#3159=VERTEX_POINT('',#10935);
#3160=VERTEX_POINT('',#10937);
#3161=VERTEX_POINT('',#10940);
#3162=VERTEX_POINT('',#10944);
#3163=VERTEX_POINT('',#10948);
#3164=VERTEX_POINT('',#10952);
#3165=VERTEX_POINT('',#10956);
#3166=VERTEX_POINT('',#10960);
#3167=VERTEX_POINT('',#10962);
#3168=VERTEX_POINT('',#10966);
#3169=VERTEX_POINT('',#10970);
#3170=VERTEX_POINT('',#10979);
#3171=VERTEX_POINT('',#10981);
#3172=VERTEX_POINT('',#10985);
#3173=VERTEX_POINT('',#10988);
#3174=VERTEX_POINT('',#10994);
#3175=VERTEX_POINT('',#10996);
#3176=VERTEX_POINT('',#11000);
#3177=VERTEX_POINT('',#11003);
#3178=VERTEX_POINT('',#11009);
#3179=VERTEX_POINT('',#11011);
#3180=EDGE_CURVE('',#2682,#2682,#2276,.T.);
#3181=EDGE_CURVE('',#2682,#2683,#1558,.T.);
#3182=EDGE_CURVE('',#2683,#2683,#2277,.T.);
#3183=EDGE_CURVE('',#2684,#2684,#2278,.F.);
#3184=EDGE_CURVE('',#2684,#2685,#1559,.T.);
#3185=EDGE_CURVE('',#2685,#2686,#2279,.F.);
#3186=EDGE_CURVE('',#2686,#2685,#2280,.F.);
#3187=EDGE_CURVE('',#2687,#2687,#2281,.F.);
#3188=EDGE_CURVE('',#2687,#2686,#1560,.T.);
#3189=EDGE_CURVE('',#2688,#2689,#2282,.F.);
#3190=EDGE_CURVE('',#2689,#2684,#1561,.T.);
#3191=EDGE_CURVE('',#2689,#2688,#2283,.F.);
#3192=EDGE_CURVE('',#2690,#2690,#2284,.F.);
#3193=EDGE_CURVE('',#2690,#2687,#1562,.T.);
#3194=EDGE_CURVE('',#2688,#2691,#1563,.T.);
#3195=EDGE_CURVE('',#2691,#2691,#2285,.T.);
#3196=EDGE_CURVE('',#2692,#2692,#2286,.T.);
#3197=EDGE_CURVE('',#2693,#2693,#2287,.T.);
#3198=EDGE_CURVE('',#2694,#2694,#2288,.T.);
#3199=EDGE_CURVE('',#2694,#2692,#1564,.T.);
#3200=EDGE_CURVE('',#2693,#2695,#1565,.T.);
#3201=EDGE_CURVE('',#2695,#2695,#2289,.F.);
#3202=EDGE_CURVE('',#2696,#2696,#2290,.F.);
#3203=EDGE_CURVE('',#2697,#2697,#2291,.F.);
#3204=EDGE_CURVE('',#2698,#2698,#2292,.F.);
#3205=EDGE_CURVE('',#2699,#2699,#2293,.F.);
#3206=EDGE_CURVE('',#2700,#2700,#2294,.F.);
#3207=EDGE_CURVE('',#2701,#2701,#2295,.F.);
#3208=EDGE_CURVE('',#2702,#2702,#2296,.T.);
#3209=EDGE_CURVE('',#2703,#2703,#2297,.F.);
#3210=EDGE_CURVE('',#2704,#2704,#2298,.F.);
#3211=EDGE_CURVE('',#2705,#2705,#2299,.F.);
#3212=EDGE_CURVE('',#2706,#2706,#2300,.F.);
#3213=EDGE_CURVE('',#2707,#2707,#2301,.F.);
#3214=EDGE_CURVE('',#2708,#2708,#2302,.F.);
#3215=EDGE_CURVE('',#2709,#2709,#2303,.T.);
#3216=EDGE_CURVE('',#2710,#2710,#2304,.F.);
#3217=EDGE_CURVE('',#2710,#2702,#1566,.T.);
#3218=EDGE_CURVE('',#2701,#2708,#1567,.T.);
#3219=EDGE_CURVE('',#2700,#2707,#1568,.T.);
#3220=EDGE_CURVE('',#2699,#2706,#1569,.T.);
#3221=EDGE_CURVE('',#2698,#2705,#1570,.T.);
#3222=EDGE_CURVE('',#2697,#2704,#1571,.T.);
#3223=EDGE_CURVE('',#2696,#2703,#1572,.T.);
#3224=EDGE_CURVE('',#2709,#2711,#1573,.T.);
#3225=EDGE_CURVE('',#2711,#2711,#2305,.T.);
#3226=EDGE_CURVE('',#2712,#2713,#2306,.T.);
#3227=EDGE_CURVE('',#2713,#2714,#2307,.T.);
#3228=EDGE_CURVE('',#2714,#2715,#2308,.F.);
#3229=EDGE_CURVE('',#2715,#2712,#2309,.T.);
#3230=EDGE_CURVE('',#2713,#2712,#2310,.T.);
#3231=EDGE_CURVE('',#2715,#2714,#2311,.T.);
#3232=EDGE_CURVE('',#2716,#2717,#2312,.F.);
#3233=EDGE_CURVE('',#2717,#2716,#2313,.F.);
#3234=EDGE_CURVE('',#2716,#2714,#1574,.T.);
#3235=EDGE_CURVE('',#2718,#2718,#2314,.T.);
#3236=EDGE_CURVE('',#2716,#2719,#2315,.T.);
#3237=EDGE_CURVE('',#2719,#2720,#2316,.F.);
#3238=EDGE_CURVE('',#2720,#2717,#2317,.T.);
#3239=EDGE_CURVE('',#2718,#2721,#1575,.T.);
#3240=EDGE_CURVE('',#2722,#2721,#2318,.F.);
#3241=EDGE_CURVE('',#2721,#2722,#2319,.F.);
#3242=EDGE_CURVE('',#2720,#2719,#2320,.F.);
#3243=EDGE_CURVE('',#2723,#2723,#2321,.F.);
#3244=EDGE_CURVE('',#2722,#2724,#2322,.T.);
#3245=EDGE_CURVE('',#2724,#2725,#2323,.T.);
#3246=EDGE_CURVE('',#2725,#2724,#2324,.T.);
#3247=EDGE_CURVE('',#2726,#2727,#2325,.F.);
#3248=EDGE_CURVE('',#2727,#2726,#2326,.F.);
#3249=EDGE_CURVE('',#2727,#2723,#1576,.T.);
#3250=EDGE_CURVE('',#2725,#2728,#1577,.T.);
#3251=EDGE_CURVE('',#2728,#2728,#2327,.T.);
#3252=EDGE_CURVE('',#2729,#2730,#2328,.T.);
#3253=EDGE_CURVE('',#2730,#2726,#2329,.T.);
#3254=EDGE_CURVE('',#2730,#2729,#2330,.T.);
#3255=EDGE_CURVE('',#2731,#2732,#2331,.T.);
#3256=EDGE_CURVE('',#2732,#2731,#2332,.T.);
#3257=EDGE_CURVE('',#2733,#2733,#2333,.F.);
#3258=EDGE_CURVE('',#2733,#2729,#1578,.T.);
#3259=EDGE_CURVE('',#2732,#2734,#2334,.T.);
#3260=EDGE_CURVE('',#2734,#2735,#2335,.T.);
#3261=EDGE_CURVE('',#2735,#2731,#2336,.T.);
#3262=EDGE_CURVE('',#2735,#2734,#2337,.T.);
#3263=EDGE_CURVE('',#2736,#2737,#2338,.F.);
#3264=EDGE_CURVE('',#2737,#2736,#2339,.F.);
#3265=EDGE_CURVE('',#2734,#2738,#1579,.T.);
#3266=EDGE_CURVE('',#2739,#2738,#2340,.F.);
#3267=EDGE_CURVE('',#2738,#2739,#2341,.F.);
#3268=EDGE_CURVE('',#2738,#2736,#2342,.T.);
#3269=EDGE_CURVE('',#2737,#2739,#2343,.T.);
#3270=EDGE_CURVE('',#2740,#2741,#2344,.T.);
#3271=EDGE_CURVE('',#2741,#2742,#2345,.T.);
#3272=EDGE_CURVE('',#2742,#2743,#2346,.F.);
#3273=EDGE_CURVE('',#2743,#2740,#2347,.T.);
#3274=EDGE_CURVE('',#2741,#2740,#2348,.T.);
#3275=EDGE_CURVE('',#2743,#2742,#2349,.T.);
#3276=EDGE_CURVE('',#2744,#2745,#2350,.F.);
#3277=EDGE_CURVE('',#2745,#2744,#2351,.F.);
#3278=EDGE_CURVE('',#2744,#2742,#1580,.T.);
#3279=EDGE_CURVE('',#2746,#2746,#2352,.T.);
#3280=EDGE_CURVE('',#2744,#2747,#2353,.T.);
#3281=EDGE_CURVE('',#2747,#2748,#2354,.F.);
#3282=EDGE_CURVE('',#2748,#2745,#2355,.T.);
#3283=EDGE_CURVE('',#2746,#2749,#1581,.T.);
#3284=EDGE_CURVE('',#2750,#2749,#2356,.F.);
#3285=EDGE_CURVE('',#2749,#2750,#2357,.F.);
#3286=EDGE_CURVE('',#2748,#2747,#2358,.F.);
#3287=EDGE_CURVE('',#2751,#2751,#2359,.F.);
#3288=EDGE_CURVE('',#2750,#2752,#2360,.T.);
#3289=EDGE_CURVE('',#2752,#2753,#2361,.T.);
#3290=EDGE_CURVE('',#2753,#2752,#2362,.T.);
#3291=EDGE_CURVE('',#2754,#2755,#2363,.F.);
#3292=EDGE_CURVE('',#2755,#2754,#2364,.F.);
#3293=EDGE_CURVE('',#2755,#2751,#1582,.T.);
#3294=EDGE_CURVE('',#2753,#2756,#1583,.T.);
#3295=EDGE_CURVE('',#2756,#2756,#2365,.T.);
#3296=EDGE_CURVE('',#2757,#2758,#2366,.T.);
#3297=EDGE_CURVE('',#2758,#2754,#2367,.T.);
#3298=EDGE_CURVE('',#2758,#2757,#2368,.T.);
#3299=EDGE_CURVE('',#2759,#2760,#2369,.T.);
#3300=EDGE_CURVE('',#2760,#2759,#2370,.T.);
#3301=EDGE_CURVE('',#2761,#2761,#2371,.F.);
#3302=EDGE_CURVE('',#2761,#2757,#1584,.T.);
#3303=EDGE_CURVE('',#2760,#2762,#2372,.T.);
#3304=EDGE_CURVE('',#2762,#2763,#2373,.T.);
#3305=EDGE_CURVE('',#2763,#2759,#2374,.T.);
#3306=EDGE_CURVE('',#2763,#2762,#2375,.T.);
#3307=EDGE_CURVE('',#2764,#2765,#2376,.F.);
#3308=EDGE_CURVE('',#2765,#2764,#2377,.F.);
#3309=EDGE_CURVE('',#2762,#2766,#1585,.T.);
#3310=EDGE_CURVE('',#2767,#2766,#2378,.F.);
#3311=EDGE_CURVE('',#2766,#2767,#2379,.F.);
#3312=EDGE_CURVE('',#2766,#2764,#2380,.T.);
#3313=EDGE_CURVE('',#2765,#2767,#2381,.T.);
#3314=EDGE_CURVE('',#2768,#2768,#2382,.F.);
#3315=EDGE_CURVE('',#2768,#2769,#1586,.T.);
#3316=EDGE_CURVE('',#2769,#2770,#2383,.F.);
#3317=EDGE_CURVE('',#2770,#2769,#2384,.F.);
#3318=EDGE_CURVE('',#2771,#2771,#2385,.F.);
#3319=EDGE_CURVE('',#2771,#2770,#1587,.T.);
#3320=EDGE_CURVE('',#2772,#2773,#2386,.F.);
#3321=EDGE_CURVE('',#2773,#2768,#1588,.T.);
#3322=EDGE_CURVE('',#2773,#2772,#2387,.F.);
#3323=EDGE_CURVE('',#2774,#2774,#2388,.F.);
#3324=EDGE_CURVE('',#2774,#2771,#1589,.T.);
#3325=EDGE_CURVE('',#2772,#2775,#1590,.T.);
#3326=EDGE_CURVE('',#2775,#2775,#2389,.T.);
#3327=EDGE_CURVE('',#2776,#2776,#2390,.T.);
#3328=EDGE_CURVE('',#2777,#2777,#2391,.T.);
#3329=EDGE_CURVE('',#2778,#2778,#2392,.T.);
#3330=EDGE_CURVE('',#2778,#2776,#1591,.T.);
#3331=EDGE_CURVE('',#2777,#2779,#1592,.T.);
#3332=EDGE_CURVE('',#2779,#2779,#2393,.F.);
#3333=EDGE_CURVE('',#2780,#2780,#2394,.F.);
#3334=EDGE_CURVE('',#2781,#2781,#2395,.F.);
#3335=EDGE_CURVE('',#2782,#2782,#2396,.F.);
#3336=EDGE_CURVE('',#2783,#2783,#2397,.F.);
#3337=EDGE_CURVE('',#2784,#2784,#2398,.F.);
#3338=EDGE_CURVE('',#2785,#2785,#2399,.F.);
#3339=EDGE_CURVE('',#2786,#2786,#2400,.T.);
#3340=EDGE_CURVE('',#2787,#2787,#2401,.F.);
#3341=EDGE_CURVE('',#2788,#2788,#2402,.F.);
#3342=EDGE_CURVE('',#2789,#2789,#2403,.F.);
#3343=EDGE_CURVE('',#2790,#2790,#2404,.F.);
#3344=EDGE_CURVE('',#2791,#2791,#2405,.F.);
#3345=EDGE_CURVE('',#2792,#2792,#2406,.F.);
#3346=EDGE_CURVE('',#2793,#2793,#2407,.T.);
#3347=EDGE_CURVE('',#2794,#2794,#2408,.F.);
#3348=EDGE_CURVE('',#2794,#2786,#1593,.T.);
#3349=EDGE_CURVE('',#2785,#2792,#1594,.T.);
#3350=EDGE_CURVE('',#2784,#2791,#1595,.T.);
#3351=EDGE_CURVE('',#2783,#2790,#1596,.T.);
#3352=EDGE_CURVE('',#2782,#2789,#1597,.T.);
#3353=EDGE_CURVE('',#2781,#2788,#1598,.T.);
#3354=EDGE_CURVE('',#2780,#2787,#1599,.T.);
#3355=EDGE_CURVE('',#2793,#2795,#1600,.T.);
#3356=EDGE_CURVE('',#2795,#2795,#2409,.T.);
#3357=EDGE_CURVE('',#2796,#2796,#2410,.T.);
#3358=EDGE_CURVE('',#2797,#2797,#2411,.T.);
#3359=EDGE_CURVE('',#2797,#2796,#1601,.T.);
#3360=EDGE_CURVE('',#2798,#2799,#2412,.F.);
#3361=EDGE_CURVE('',#2800,#2798,#1602,.F.);
#3362=EDGE_CURVE('',#2801,#2800,#2413,.F.);
#3363=EDGE_CURVE('',#2799,#2801,#1603,.F.);
#3364=EDGE_CURVE('',#2802,#2801,#1604,.T.);
#3365=EDGE_CURVE('',#2803,#2802,#1605,.T.);
#3366=EDGE_CURVE('',#2799,#2803,#1606,.T.);
#3367=EDGE_CURVE('',#2804,#2800,#1607,.F.);
#3368=EDGE_CURVE('',#2805,#2804,#2414,.F.);
#3369=EDGE_CURVE('',#2801,#2805,#1608,.F.);
#3370=EDGE_CURVE('',#2806,#2807,#2415,.F.);
#3371=EDGE_CURVE('',#2798,#2806,#1609,.F.);
#3372=EDGE_CURVE('',#2807,#2799,#1610,.F.);
#3373=EDGE_CURVE('',#2808,#2805,#1611,.T.);
#3374=EDGE_CURVE('',#2802,#2808,#1612,.T.);
#3375=EDGE_CURVE('',#2809,#2810,#1613,.F.);
#3376=EDGE_CURVE('',#2803,#2809,#2416,.F.);
#3377=EDGE_CURVE('',#2810,#2802,#2417,.F.);
#3378=EDGE_CURVE('',#2807,#2811,#1614,.T.);
#3379=EDGE_CURVE('',#2811,#2803,#1615,.T.);
#3380=EDGE_CURVE('',#2804,#2806,#1616,.F.);
#3381=EDGE_CURVE('',#2807,#2805,#1617,.F.);
#3382=EDGE_CURVE('',#2800,#2810,#1618,.T.);
#3383=EDGE_CURVE('',#2809,#2798,#1619,.T.);
#3384=EDGE_CURVE('',#2812,#2806,#1620,.T.);
#3385=EDGE_CURVE('',#2809,#2812,#1621,.T.);
#3386=EDGE_CURVE('',#2808,#2811,#1622,.T.);
#3387=EDGE_CURVE('',#2813,#2808,#2418,.F.);
#3388=EDGE_CURVE('',#2810,#2813,#1623,.F.);
#3389=EDGE_CURVE('',#2811,#2812,#2419,.F.);
#3390=EDGE_CURVE('',#2804,#2813,#1624,.T.);
#3391=EDGE_CURVE('',#2812,#2813,#1625,.T.);
#3392=EDGE_CURVE('',#2814,#2814,#2420,.T.);
#3393=EDGE_CURVE('',#2814,#2815,#1626,.T.);
#3394=EDGE_CURVE('',#2815,#2815,#2421,.F.);
#3395=EDGE_CURVE('',#2816,#2817,#1627,.T.);
#3396=EDGE_CURVE('',#2818,#2816,#1628,.T.);
#3397=EDGE_CURVE('',#2819,#2818,#1629,.T.);
#3398=EDGE_CURVE('',#2817,#2819,#1630,.T.);
#3399=EDGE_CURVE('',#2820,#2820,#2422,.T.);
#3400=EDGE_CURVE('',#2821,#2821,#2423,.T.);
#3401=EDGE_CURVE('',#2822,#2822,#2424,.T.);
#3402=EDGE_CURVE('',#2823,#2823,#2425,.T.);
#3403=EDGE_CURVE('',#2824,#2825,#1631,.T.);
#3404=EDGE_CURVE('',#2825,#2826,#1632,.T.);
#3405=EDGE_CURVE('',#2826,#2827,#1633,.T.);
#3406=EDGE_CURVE('',#2827,#2824,#1634,.T.);
#3407=EDGE_CURVE('',#2828,#2828,#2426,.T.);
#3408=EDGE_CURVE('',#2829,#2829,#2427,.T.);
#3409=EDGE_CURVE('',#2830,#2830,#2428,.T.);
#3410=EDGE_CURVE('',#2831,#2831,#2429,.T.);
#3411=EDGE_CURVE('',#2831,#2823,#1635,.T.);
#3412=EDGE_CURVE('',#2828,#2822,#1636,.T.);
#3413=EDGE_CURVE('',#2829,#2821,#1637,.T.);
#3414=EDGE_CURVE('',#2830,#2820,#1638,.T.);
#3415=EDGE_CURVE('',#2818,#2824,#1639,.T.);
#3416=EDGE_CURVE('',#2825,#2816,#1640,.T.);
#3417=EDGE_CURVE('',#2827,#2819,#1641,.T.);
#3418=EDGE_CURVE('',#2826,#2817,#1642,.T.);
#3419=EDGE_CURVE('',#2832,#2833,#2430,.T.);
#3420=EDGE_CURVE('',#2833,#2834,#2431,.T.);
#3421=EDGE_CURVE('',#2834,#2835,#2432,.F.);
#3422=EDGE_CURVE('',#2835,#2832,#2433,.T.);
#3423=EDGE_CURVE('',#2833,#2832,#2434,.T.);
#3424=EDGE_CURVE('',#2835,#2834,#2435,.T.);
#3425=EDGE_CURVE('',#2836,#2837,#2436,.F.);
#3426=EDGE_CURVE('',#2837,#2836,#2437,.F.);
#3427=EDGE_CURVE('',#2836,#2834,#1643,.T.);
#3428=EDGE_CURVE('',#2838,#2838,#2438,.T.);
#3429=EDGE_CURVE('',#2836,#2839,#2439,.T.);
#3430=EDGE_CURVE('',#2839,#2840,#2440,.F.);
#3431=EDGE_CURVE('',#2840,#2837,#2441,.T.);
#3432=EDGE_CURVE('',#2838,#2841,#1644,.T.);
#3433=EDGE_CURVE('',#2842,#2841,#2442,.F.);
#3434=EDGE_CURVE('',#2841,#2842,#2443,.F.);
#3435=EDGE_CURVE('',#2840,#2839,#2444,.F.);
#3436=EDGE_CURVE('',#2843,#2843,#2445,.F.);
#3437=EDGE_CURVE('',#2842,#2844,#2446,.T.);
#3438=EDGE_CURVE('',#2844,#2845,#2447,.T.);
#3439=EDGE_CURVE('',#2845,#2844,#2448,.T.);
#3440=EDGE_CURVE('',#2846,#2847,#2449,.F.);
#3441=EDGE_CURVE('',#2847,#2846,#2450,.F.);
#3442=EDGE_CURVE('',#2847,#2843,#1645,.T.);
#3443=EDGE_CURVE('',#2845,#2848,#1646,.T.);
#3444=EDGE_CURVE('',#2848,#2848,#2451,.T.);
#3445=EDGE_CURVE('',#2849,#2850,#2452,.T.);
#3446=EDGE_CURVE('',#2850,#2846,#2453,.T.);
#3447=EDGE_CURVE('',#2850,#2849,#2454,.T.);
#3448=EDGE_CURVE('',#2851,#2852,#2455,.T.);
#3449=EDGE_CURVE('',#2852,#2851,#2456,.T.);
#3450=EDGE_CURVE('',#2853,#2853,#2457,.F.);
#3451=EDGE_CURVE('',#2853,#2849,#1647,.T.);
#3452=EDGE_CURVE('',#2852,#2854,#2458,.T.);
#3453=EDGE_CURVE('',#2854,#2855,#2459,.T.);
#3454=EDGE_CURVE('',#2855,#2851,#2460,.T.);
#3455=EDGE_CURVE('',#2855,#2854,#2461,.T.);
#3456=EDGE_CURVE('',#2856,#2857,#2462,.F.);
#3457=EDGE_CURVE('',#2857,#2856,#2463,.F.);
#3458=EDGE_CURVE('',#2854,#2858,#1648,.T.);
#3459=EDGE_CURVE('',#2859,#2858,#2464,.F.);
#3460=EDGE_CURVE('',#2858,#2859,#2465,.F.);
#3461=EDGE_CURVE('',#2858,#2856,#2466,.T.);
#3462=EDGE_CURVE('',#2857,#2859,#2467,.T.);
#3463=EDGE_CURVE('',#2860,#2860,#2468,.F.);
#3464=EDGE_CURVE('',#2860,#2861,#1649,.T.);
#3465=EDGE_CURVE('',#2861,#2861,#2469,.T.);
#3466=EDGE_CURVE('',#2862,#2862,#2470,.F.);
#3467=EDGE_CURVE('',#2863,#2864,#2471,.T.);
#3468=EDGE_CURVE('',#2865,#2863,#1650,.T.);
#3469=EDGE_CURVE('',#2866,#2865,#1651,.T.);
#3470=EDGE_CURVE('',#2864,#2866,#2472,.F.);
#3471=EDGE_CURVE('',#2867,#2867,#2473,.T.);
#3472=EDGE_CURVE('',#2868,#2868,#2474,.T.);
#3473=EDGE_CURVE('',#2869,#2869,#2475,.T.);
#3474=EDGE_CURVE('',#2870,#2870,#2476,.T.);
#3475=EDGE_CURVE('',#2871,#2871,#2477,.T.);
#3476=EDGE_CURVE('',#2871,#2862,#1652,.T.);
#3477=EDGE_CURVE('',#2872,#2872,#2478,.T.);
#3478=EDGE_CURVE('',#2872,#2870,#1653,.T.);
#3479=EDGE_CURVE('',#2873,#2873,#2479,.T.);
#3480=EDGE_CURVE('',#2873,#2869,#1654,.T.);
#3481=EDGE_CURVE('',#2874,#2874,#2480,.T.);
#3482=EDGE_CURVE('',#2874,#2868,#1655,.T.);
#3483=EDGE_CURVE('',#2875,#2875,#2481,.T.);
#3484=EDGE_CURVE('',#2875,#2867,#1656,.T.);
#3485=EDGE_CURVE('',#2865,#2876,#1657,.T.);
#3486=EDGE_CURVE('',#2877,#2863,#1658,.T.);
#3487=EDGE_CURVE('',#2876,#2877,#1659,.T.);
#3488=EDGE_CURVE('',#2876,#2878,#1660,.T.);
#3489=EDGE_CURVE('',#2878,#2866,#1661,.T.);
#3490=EDGE_CURVE('',#2879,#2864,#1662,.F.);
#3491=EDGE_CURVE('',#2878,#2879,#2482,.T.);
#3492=EDGE_CURVE('',#2877,#2879,#2483,.T.);
#3493=EDGE_CURVE('',#2880,#2881,#2484,.T.);
#3494=EDGE_CURVE('',#2881,#2882,#2485,.T.);
#3495=EDGE_CURVE('',#2882,#2883,#2486,.F.);
#3496=EDGE_CURVE('',#2883,#2880,#2487,.T.);
#3497=EDGE_CURVE('',#2881,#2880,#2488,.T.);
#3498=EDGE_CURVE('',#2883,#2882,#2489,.T.);
#3499=EDGE_CURVE('',#2884,#2885,#2490,.F.);
#3500=EDGE_CURVE('',#2885,#2884,#2491,.F.);
#3501=EDGE_CURVE('',#2884,#2882,#1663,.T.);
#3502=EDGE_CURVE('',#2886,#2886,#2492,.T.);
#3503=EDGE_CURVE('',#2884,#2887,#2493,.T.);
#3504=EDGE_CURVE('',#2887,#2888,#2494,.F.);
#3505=EDGE_CURVE('',#2888,#2885,#2495,.T.);
#3506=EDGE_CURVE('',#2886,#2889,#1664,.T.);
#3507=EDGE_CURVE('',#2890,#2889,#2496,.F.);
#3508=EDGE_CURVE('',#2889,#2890,#2497,.F.);
#3509=EDGE_CURVE('',#2888,#2887,#2498,.F.);
#3510=EDGE_CURVE('',#2891,#2891,#2499,.F.);
#3511=EDGE_CURVE('',#2890,#2892,#2500,.T.);
#3512=EDGE_CURVE('',#2892,#2893,#2501,.T.);
#3513=EDGE_CURVE('',#2893,#2892,#2502,.T.);
#3514=EDGE_CURVE('',#2894,#2895,#2503,.F.);
#3515=EDGE_CURVE('',#2895,#2894,#2504,.F.);
#3516=EDGE_CURVE('',#2895,#2891,#1665,.T.);
#3517=EDGE_CURVE('',#2893,#2896,#1666,.T.);
#3518=EDGE_CURVE('',#2896,#2896,#2505,.T.);
#3519=EDGE_CURVE('',#2897,#2898,#2506,.T.);
#3520=EDGE_CURVE('',#2898,#2894,#2507,.T.);
#3521=EDGE_CURVE('',#2898,#2897,#2508,.T.);
#3522=EDGE_CURVE('',#2899,#2900,#2509,.T.);
#3523=EDGE_CURVE('',#2900,#2899,#2510,.T.);
#3524=EDGE_CURVE('',#2901,#2901,#2511,.F.);
#3525=EDGE_CURVE('',#2901,#2897,#1667,.T.);
#3526=EDGE_CURVE('',#2900,#2902,#2512,.T.);
#3527=EDGE_CURVE('',#2902,#2903,#2513,.T.);
#3528=EDGE_CURVE('',#2903,#2899,#2514,.T.);
#3529=EDGE_CURVE('',#2903,#2902,#2515,.T.);
#3530=EDGE_CURVE('',#2904,#2905,#2516,.F.);
#3531=EDGE_CURVE('',#2905,#2904,#2517,.F.);
#3532=EDGE_CURVE('',#2902,#2906,#1668,.T.);
#3533=EDGE_CURVE('',#2907,#2906,#2518,.F.);
#3534=EDGE_CURVE('',#2906,#2907,#2519,.F.);
#3535=EDGE_CURVE('',#2906,#2904,#2520,.T.);
#3536=EDGE_CURVE('',#2905,#2907,#2521,.T.);
#3537=EDGE_CURVE('',#2908,#2908,#2522,.T.);
#3538=EDGE_CURVE('',#2908,#2909,#1669,.T.);
#3539=EDGE_CURVE('',#2909,#2909,#2523,.F.);
#3540=EDGE_CURVE('',#2910,#2910,#2524,.T.);
#3541=EDGE_CURVE('',#2911,#2911,#2525,.F.);
#3542=EDGE_CURVE('',#2911,#2910,#1670,.T.);
#3543=EDGE_CURVE('',#2912,#2913,#2526,.F.);
#3544=EDGE_CURVE('',#2913,#2914,#2527,.F.);
#3545=EDGE_CURVE('',#2914,#2915,#2528,.F.);
#3546=EDGE_CURVE('',#2915,#2916,#2529,.F.);
#3547=EDGE_CURVE('',#2916,#2917,#1671,.T.);
#3548=EDGE_CURVE('',#2917,#2917,#2530,.T.);
#3549=EDGE_CURVE('',#2916,#2918,#2531,.F.);
#3550=EDGE_CURVE('',#2918,#2919,#2532,.F.);
#3551=EDGE_CURVE('',#2919,#2912,#2533,.F.);
#3552=EDGE_CURVE('',#2915,#2918,#1672,.T.);
#3553=EDGE_CURVE('',#2920,#2919,#1673,.T.);
#3554=EDGE_CURVE('',#2918,#2920,#1674,.T.);
#3555=EDGE_CURVE('',#2921,#2912,#1675,.T.);
#3556=EDGE_CURVE('',#2919,#2921,#1676,.T.);
#3557=EDGE_CURVE('',#2912,#2913,#1677,.T.);
#3558=EDGE_CURVE('',#2922,#2914,#1678,.T.);
#3559=EDGE_CURVE('',#2913,#2922,#1679,.T.);
#3560=EDGE_CURVE('',#2923,#2915,#1680,.T.);
#3561=EDGE_CURVE('',#2914,#2923,#1681,.T.);
#3562=EDGE_CURVE('',#2924,#2923,#1682,.T.);
#3563=EDGE_CURVE('',#2925,#2924,#1683,.T.);
#3564=EDGE_CURVE('',#2920,#2925,#1684,.T.);
#3565=EDGE_CURVE('',#2926,#2925,#1685,.T.);
#3566=EDGE_CURVE('',#2921,#2926,#1686,.T.);
#3567=EDGE_CURVE('',#2926,#2927,#1687,.T.);
#3568=EDGE_CURVE('',#2927,#2922,#1688,.T.);
#3569=EDGE_CURVE('',#2927,#2924,#1689,.T.);
#3570=EDGE_CURVE('',#2928,#2928,#2534,.T.);
#3571=EDGE_CURVE('',#2928,#2929,#1690,.T.);
#3572=EDGE_CURVE('',#2929,#2929,#2535,.F.);
#3573=EDGE_CURVE('',#2930,#2930,#2536,.T.);
#3574=EDGE_CURVE('',#2931,#2931,#2537,.F.);
#3575=EDGE_CURVE('',#2931,#2930,#1691,.T.);
#3576=EDGE_CURVE('',#2932,#2933,#2538,.F.);
#3577=EDGE_CURVE('',#2933,#2934,#2539,.F.);
#3578=EDGE_CURVE('',#2934,#2935,#2540,.F.);
#3579=EDGE_CURVE('',#2935,#2936,#2541,.F.);
#3580=EDGE_CURVE('',#2936,#2937,#1692,.T.);
#3581=EDGE_CURVE('',#2937,#2937,#2542,.T.);
#3582=EDGE_CURVE('',#2936,#2938,#2543,.F.);
#3583=EDGE_CURVE('',#2938,#2939,#2544,.F.);
#3584=EDGE_CURVE('',#2939,#2932,#2545,.F.);
#3585=EDGE_CURVE('',#2935,#2938,#1693,.T.);
#3586=EDGE_CURVE('',#2940,#2939,#1694,.T.);
#3587=EDGE_CURVE('',#2938,#2940,#1695,.T.);
#3588=EDGE_CURVE('',#2941,#2932,#1696,.T.);
#3589=EDGE_CURVE('',#2939,#2941,#1697,.T.);
#3590=EDGE_CURVE('',#2932,#2933,#1698,.T.);
#3591=EDGE_CURVE('',#2942,#2934,#1699,.T.);
#3592=EDGE_CURVE('',#2933,#2942,#1700,.T.);
#3593=EDGE_CURVE('',#2943,#2935,#1701,.T.);
#3594=EDGE_CURVE('',#2934,#2943,#1702,.T.);
#3595=EDGE_CURVE('',#2944,#2943,#1703,.T.);
#3596=EDGE_CURVE('',#2945,#2944,#1704,.T.);
#3597=EDGE_CURVE('',#2940,#2945,#1705,.T.);
#3598=EDGE_CURVE('',#2946,#2945,#1706,.T.);
#3599=EDGE_CURVE('',#2941,#2946,#1707,.T.);
#3600=EDGE_CURVE('',#2946,#2947,#1708,.T.);
#3601=EDGE_CURVE('',#2947,#2942,#1709,.T.);
#3602=EDGE_CURVE('',#2947,#2944,#1710,.T.);
#3603=EDGE_CURVE('',#2948,#2949,#2546,.F.);
#3604=EDGE_CURVE('',#2949,#2950,#2547,.F.);
#3605=EDGE_CURVE('',#2950,#2951,#2548,.F.);
#3606=EDGE_CURVE('',#2951,#2952,#2549,.F.);
#3607=EDGE_CURVE('',#2952,#2953,#1711,.T.);
#3608=EDGE_CURVE('',#2953,#2953,#2550,.T.);
#3609=EDGE_CURVE('',#2952,#2954,#2551,.F.);
#3610=EDGE_CURVE('',#2954,#2955,#2552,.F.);
#3611=EDGE_CURVE('',#2955,#2948,#2553,.F.);
#3612=EDGE_CURVE('',#2951,#2954,#1712,.T.);
#3613=EDGE_CURVE('',#2956,#2955,#1713,.T.);
#3614=EDGE_CURVE('',#2954,#2956,#1714,.T.);
#3615=EDGE_CURVE('',#2957,#2948,#1715,.T.);
#3616=EDGE_CURVE('',#2955,#2957,#1716,.T.);
#3617=EDGE_CURVE('',#2948,#2949,#1717,.T.);
#3618=EDGE_CURVE('',#2958,#2950,#1718,.T.);
#3619=EDGE_CURVE('',#2949,#2958,#1719,.T.);
#3620=EDGE_CURVE('',#2959,#2951,#1720,.T.);
#3621=EDGE_CURVE('',#2950,#2959,#1721,.T.);
#3622=EDGE_CURVE('',#2960,#2959,#1722,.T.);
#3623=EDGE_CURVE('',#2961,#2960,#1723,.T.);
#3624=EDGE_CURVE('',#2956,#2961,#1724,.T.);
#3625=EDGE_CURVE('',#2962,#2961,#1725,.T.);
#3626=EDGE_CURVE('',#2957,#2962,#1726,.T.);
#3627=EDGE_CURVE('',#2962,#2963,#1727,.T.);
#3628=EDGE_CURVE('',#2963,#2958,#1728,.T.);
#3629=EDGE_CURVE('',#2963,#2960,#1729,.T.);
#3630=EDGE_CURVE('',#2964,#2964,#2554,.T.);
#3631=EDGE_CURVE('',#2964,#2965,#1730,.T.);
#3632=EDGE_CURVE('',#2965,#2965,#2555,.F.);
#3633=EDGE_CURVE('',#2966,#2966,#2556,.T.);
#3634=EDGE_CURVE('',#2967,#2967,#2557,.F.);
#3635=EDGE_CURVE('',#2967,#2966,#1731,.T.);
#3636=EDGE_CURVE('',#2968,#2969,#2558,.T.);
#3637=EDGE_CURVE('',#2968,#2970,#1732,.T.);
#3638=EDGE_CURVE('',#2971,#2970,#2559,.F.);
#3639=EDGE_CURVE('',#2970,#2971,#2560,.F.);
#3640=EDGE_CURVE('',#2969,#2968,#2561,.T.);
#3641=EDGE_CURVE('',#2972,#2972,#2562,.T.);
#3642=EDGE_CURVE('',#2972,#2973,#1733,.T.);
#3643=EDGE_CURVE('',#2974,#2973,#2563,.F.);
#3644=EDGE_CURVE('',#2973,#2974,#2564,.F.);
#3645=EDGE_CURVE('',#2975,#2976,#2565,.T.);
#3646=EDGE_CURVE('',#2975,#2977,#1734,.T.);
#3647=EDGE_CURVE('',#2977,#2977,#2566,.T.);
#3648=EDGE_CURVE('',#2976,#2975,#2567,.T.);
#3649=EDGE_CURVE('',#2978,#2978,#2568,.F.);
#3650=EDGE_CURVE('',#2978,#2979,#1735,.T.);
#3651=EDGE_CURVE('',#2979,#2979,#2569,.T.);
#3652=EDGE_CURVE('',#2980,#2980,#2570,.T.);
#3653=EDGE_CURVE('',#2980,#2981,#1736,.T.);
#3654=EDGE_CURVE('',#2981,#2981,#2571,.T.);
#3655=EDGE_CURVE('',#2982,#2982,#2572,.T.);
#3656=EDGE_CURVE('',#2974,#2969,#1737,.T.);
#3657=EDGE_CURVE('',#2983,#2983,#2573,.T.);
#3658=EDGE_CURVE('',#2983,#2982,#1738,.T.);
#3659=EDGE_CURVE('',#2971,#2976,#1739,.T.);
#3660=EDGE_CURVE('',#2978,#2981,#1740,.T.);
#3661=EDGE_CURVE('',#2984,#2984,#2574,.T.);
#3662=EDGE_CURVE('',#2984,#2985,#1741,.T.);
#3663=EDGE_CURVE('',#2985,#2985,#2575,.F.);
#3664=EDGE_CURVE('',#2986,#2987,#1742,.T.);
#3665=EDGE_CURVE('',#2988,#2986,#1743,.T.);
#3666=EDGE_CURVE('',#2989,#2988,#1744,.T.);
#3667=EDGE_CURVE('',#2987,#2989,#1745,.T.);
#3668=EDGE_CURVE('',#2990,#2990,#2576,.T.);
#3669=EDGE_CURVE('',#2991,#2991,#2577,.T.);
#3670=EDGE_CURVE('',#2992,#2992,#2578,.F.);
#3671=EDGE_CURVE('',#2993,#2993,#2579,.F.);
#3672=EDGE_CURVE('',#2994,#2994,#2580,.F.);
#3673=EDGE_CURVE('',#2995,#2995,#2581,.F.);
#3674=EDGE_CURVE('',#2996,#2996,#2582,.T.);
#3675=EDGE_CURVE('',#2997,#2997,#2583,.T.);
#3676=EDGE_CURVE('',#2998,#2999,#1746,.T.);
#3677=EDGE_CURVE('',#2999,#3000,#1747,.T.);
#3678=EDGE_CURVE('',#3000,#3001,#1748,.T.);
#3679=EDGE_CURVE('',#3001,#3002,#1749,.T.);
#3680=EDGE_CURVE('',#3002,#3003,#1750,.T.);
#3681=EDGE_CURVE('',#3003,#3004,#1751,.T.);
#3682=EDGE_CURVE('',#3004,#3005,#1752,.T.);
#3683=EDGE_CURVE('',#3005,#2998,#1753,.T.);
#3684=EDGE_CURVE('',#3006,#3006,#2584,.T.);
#3685=EDGE_CURVE('',#3007,#3007,#2585,.T.);
#3686=EDGE_CURVE('',#3008,#3008,#2586,.F.);
#3687=EDGE_CURVE('',#3009,#3009,#2587,.F.);
#3688=EDGE_CURVE('',#3010,#3010,#2588,.F.);
#3689=EDGE_CURVE('',#3011,#3011,#2589,.F.);
#3690=EDGE_CURVE('',#3012,#3012,#2590,.T.);
#3691=EDGE_CURVE('',#3013,#3013,#2591,.T.);
#3692=EDGE_CURVE('',#3013,#2997,#1754,.T.);
#3693=EDGE_CURVE('',#3006,#2996,#1755,.T.);
#3694=EDGE_CURVE('',#2995,#3011,#1756,.T.);
#3695=EDGE_CURVE('',#2994,#3010,#1757,.T.);
#3696=EDGE_CURVE('',#2993,#3009,#1758,.T.);
#3697=EDGE_CURVE('',#2992,#3008,#1759,.T.);
#3698=EDGE_CURVE('',#3007,#2991,#1760,.T.);
#3699=EDGE_CURVE('',#3012,#2990,#1761,.T.);
#3700=EDGE_CURVE('',#3014,#3015,#1762,.T.);
#3701=EDGE_CURVE('',#3016,#3014,#1763,.T.);
#3702=EDGE_CURVE('',#3017,#3016,#1764,.T.);
#3703=EDGE_CURVE('',#3001,#3017,#1765,.T.);
#3704=EDGE_CURVE('',#2988,#3000,#1766,.T.);
#3705=EDGE_CURVE('',#3015,#2986,#1767,.T.);
#3706=EDGE_CURVE('',#2989,#2999,#1768,.T.);
#3707=EDGE_CURVE('',#2987,#2998,#1769,.T.);
#3708=EDGE_CURVE('',#3018,#3005,#1770,.T.);
#3709=EDGE_CURVE('',#3019,#3018,#1771,.T.);
#3710=EDGE_CURVE('',#3020,#3019,#1772,.T.);
#3711=EDGE_CURVE('',#3015,#3020,#1773,.T.);
#3712=EDGE_CURVE('',#3021,#3004,#1774,.T.);
#3713=EDGE_CURVE('',#3018,#3021,#1775,.T.);
#3714=EDGE_CURVE('',#3003,#3022,#1776,.T.);
#3715=EDGE_CURVE('',#3022,#3021,#1777,.T.);
#3716=EDGE_CURVE('',#3002,#3023,#1778,.T.);
#3717=EDGE_CURVE('',#3023,#3022,#1779,.T.);
#3718=EDGE_CURVE('',#3017,#3023,#1780,.T.);
#3719=EDGE_CURVE('',#3024,#3025,#1781,.T.);
#3720=EDGE_CURVE('',#3016,#3024,#1782,.T.);
#3721=EDGE_CURVE('',#3025,#3014,#1783,.T.);
#3722=EDGE_CURVE('',#3019,#3024,#1784,.T.);
#3723=EDGE_CURVE('',#3026,#3026,#2592,.T.);
#3724=EDGE_CURVE('',#3027,#3027,#2593,.T.);
#3725=EDGE_CURVE('',#3028,#3028,#2594,.T.);
#3726=EDGE_CURVE('',#3029,#3029,#2595,.F.);
#3727=EDGE_CURVE('',#3030,#3030,#2596,.F.);
#3728=EDGE_CURVE('',#3031,#3031,#2597,.F.);
#3729=EDGE_CURVE('',#3032,#3032,#2598,.F.);
#3730=EDGE_CURVE('',#3033,#3033,#2599,.T.);
#3731=EDGE_CURVE('',#3034,#3034,#2600,.T.);
#3732=EDGE_CURVE('',#3020,#3025,#1785,.T.);
#3733=EDGE_CURVE('',#3035,#3035,#2601,.T.);
#3734=EDGE_CURVE('',#3036,#3036,#2602,.T.);
#3735=EDGE_CURVE('',#3037,#3037,#2603,.T.);
#3736=EDGE_CURVE('',#3038,#3038,#2604,.F.);
#3737=EDGE_CURVE('',#3039,#3039,#2605,.F.);
#3738=EDGE_CURVE('',#3040,#3040,#2606,.F.);
#3739=EDGE_CURVE('',#3041,#3041,#2607,.F.);
#3740=EDGE_CURVE('',#3042,#3042,#2608,.T.);
#3741=EDGE_CURVE('',#3043,#3043,#2609,.T.);
#3742=EDGE_CURVE('',#3043,#3034,#1786,.T.);
#3743=EDGE_CURVE('',#3036,#3033,#1787,.T.);
#3744=EDGE_CURVE('',#3032,#3041,#1788,.T.);
#3745=EDGE_CURVE('',#3031,#3040,#1789,.T.);
#3746=EDGE_CURVE('',#3030,#3039,#1790,.T.);
#3747=EDGE_CURVE('',#3029,#3038,#1791,.T.);
#3748=EDGE_CURVE('',#3037,#3028,#1792,.T.);
#3749=EDGE_CURVE('',#3042,#3027,#1793,.T.);
#3750=EDGE_CURVE('',#3035,#3026,#1794,.T.);
#3751=EDGE_CURVE('',#3044,#3044,#2610,.F.);
#3752=EDGE_CURVE('',#3044,#3045,#1795,.T.);
#3753=EDGE_CURVE('',#3045,#3045,#2611,.T.);
#3754=EDGE_CURVE('',#3046,#3046,#2612,.F.);
#3755=EDGE_CURVE('',#3047,#3047,#2613,.F.);
#3756=EDGE_CURVE('',#3047,#3046,#1796,.T.);
#3757=EDGE_CURVE('',#3048,#3048,#2614,.T.);
#3758=EDGE_CURVE('',#3049,#3049,#2615,.F.);
#3759=EDGE_CURVE('',#3049,#3048,#1797,.T.);
#3760=EDGE_CURVE('',#3050,#3050,#2616,.T.);
#3761=EDGE_CURVE('',#3050,#3051,#1798,.T.);
#3762=EDGE_CURVE('',#3051,#3051,#2617,.F.);
#3763=EDGE_CURVE('',#3052,#3053,#1799,.T.);
#3764=EDGE_CURVE('',#3053,#3054,#1800,.T.);
#3765=EDGE_CURVE('',#3054,#3055,#2618,.F.);
#3766=EDGE_CURVE('',#3055,#3052,#1801,.T.);
#3767=EDGE_CURVE('',#3056,#3056,#2619,.T.);
#3768=EDGE_CURVE('',#3056,#3057,#1802,.T.);
#3769=EDGE_CURVE('',#3057,#3057,#2620,.F.);
#3770=EDGE_CURVE('',#3058,#3055,#1803,.T.);
#3771=EDGE_CURVE('',#3059,#3058,#1804,.T.);
#3772=EDGE_CURVE('',#3052,#3059,#1805,.T.);
#3773=EDGE_CURVE('',#3054,#3060,#1806,.F.);
#3774=EDGE_CURVE('',#3060,#3058,#2621,.F.);
#3775=EDGE_CURVE('',#3061,#3053,#1807,.T.);
#3776=EDGE_CURVE('',#3060,#3061,#1808,.T.);
#3777=EDGE_CURVE('',#3061,#3059,#1809,.T.);
#3778=EDGE_CURVE('',#3062,#3063,#1810,.T.);
#3779=EDGE_CURVE('',#3064,#3062,#1811,.T.);
#3780=EDGE_CURVE('',#3065,#3064,#1812,.T.);
#3781=EDGE_CURVE('',#3063,#3065,#1813,.T.);
#3782=EDGE_CURVE('',#3066,#3062,#1814,.T.);
#3783=EDGE_CURVE('',#3067,#3066,#1815,.T.);
#3784=EDGE_CURVE('',#3064,#3067,#1816,.T.);
#3785=EDGE_CURVE('',#3068,#3067,#1817,.T.);
#3786=EDGE_CURVE('',#3065,#3068,#1818,.T.);
#3787=EDGE_CURVE('',#3063,#3069,#1819,.T.);
#3788=EDGE_CURVE('',#3069,#3066,#1820,.T.);
#3789=EDGE_CURVE('',#3068,#3069,#1821,.T.);
#3790=EDGE_CURVE('',#3070,#3070,#2622,.T.);
#3791=EDGE_CURVE('',#3070,#3071,#1822,.T.);
#3792=EDGE_CURVE('',#3071,#3071,#2623,.F.);
#3793=EDGE_CURVE('',#3072,#3073,#1823,.T.);
#3794=EDGE_CURVE('',#3073,#3074,#1824,.T.);
#3795=EDGE_CURVE('',#3074,#3075,#2624,.F.);
#3796=EDGE_CURVE('',#3075,#3072,#1825,.T.);
#3797=EDGE_CURVE('',#3076,#3076,#2625,.T.);
#3798=EDGE_CURVE('',#3076,#3077,#1826,.T.);
#3799=EDGE_CURVE('',#3077,#3077,#2626,.F.);
#3800=EDGE_CURVE('',#3078,#3075,#1827,.T.);
#3801=EDGE_CURVE('',#3079,#3078,#1828,.T.);
#3802=EDGE_CURVE('',#3072,#3079,#1829,.T.);
#3803=EDGE_CURVE('',#3074,#3080,#1830,.F.);
#3804=EDGE_CURVE('',#3080,#3078,#2627,.F.);
#3805=EDGE_CURVE('',#3081,#3073,#1831,.T.);
#3806=EDGE_CURVE('',#3080,#3081,#1832,.T.);
#3807=EDGE_CURVE('',#3081,#3079,#1833,.T.);
#3808=EDGE_CURVE('',#3082,#3082,#2628,.T.);
#3809=EDGE_CURVE('',#3082,#3083,#1834,.T.);
#3810=EDGE_CURVE('',#3083,#3083,#2629,.F.);
#3811=EDGE_CURVE('',#3084,#3085,#1835,.T.);
#3812=EDGE_CURVE('',#3086,#3084,#1836,.T.);
#3813=EDGE_CURVE('',#3087,#3086,#1837,.T.);
#3814=EDGE_CURVE('',#3088,#3087,#1838,.T.);
#3815=EDGE_CURVE('',#3089,#3088,#1839,.T.);
#3816=EDGE_CURVE('',#3085,#3089,#1840,.T.);
#3817=EDGE_CURVE('',#3090,#3090,#2630,.T.);
#3818=EDGE_CURVE('',#3091,#3091,#2631,.T.);
#3819=EDGE_CURVE('',#3092,#3093,#1841,.T.);
#3820=EDGE_CURVE('',#3094,#3092,#1842,.T.);
#3821=EDGE_CURVE('',#3095,#3094,#1843,.T.);
#3822=EDGE_CURVE('',#3096,#3095,#1844,.T.);
#3823=EDGE_CURVE('',#3086,#3096,#1845,.T.);
#3824=EDGE_CURVE('',#3097,#3084,#1846,.T.);
#3825=EDGE_CURVE('',#3093,#3097,#1847,.T.);
#3826=EDGE_CURVE('',#3098,#3096,#1848,.T.);
#3827=EDGE_CURVE('',#3087,#3098,#1849,.T.);
#3828=EDGE_CURVE('',#3099,#3098,#1850,.T.);
#3829=EDGE_CURVE('',#3088,#3099,#1851,.T.);
#3830=EDGE_CURVE('',#3100,#3099,#1852,.T.);
#3831=EDGE_CURVE('',#3089,#3100,#1853,.T.);
#3832=EDGE_CURVE('',#3101,#3102,#1854,.T.);
#3833=EDGE_CURVE('',#3103,#3101,#1855,.T.);
#3834=EDGE_CURVE('',#3104,#3103,#1856,.T.);
#3835=EDGE_CURVE('',#3105,#3104,#1857,.T.);
#3836=EDGE_CURVE('',#3085,#3105,#1858,.T.);
#3837=EDGE_CURVE('',#3102,#3100,#1859,.T.);
#3838=EDGE_CURVE('',#3101,#3094,#1860,.T.);
#3839=EDGE_CURVE('',#3092,#3103,#1861,.T.);
#3840=EDGE_CURVE('',#3106,#3106,#2632,.F.);
#3841=EDGE_CURVE('',#3095,#3102,#1862,.T.);
#3842=EDGE_CURVE('',#3107,#3107,#2633,.T.);
#3843=EDGE_CURVE('',#3097,#3105,#1863,.T.);
#3844=EDGE_CURVE('',#3093,#3104,#1864,.T.);
#3845=EDGE_CURVE('',#3108,#3108,#2634,.F.);
#3846=EDGE_CURVE('',#3109,#3109,#2635,.F.);
#3847=EDGE_CURVE('',#3109,#3091,#1865,.T.);
#3848=EDGE_CURVE('',#3108,#3090,#1866,.T.);
#3849=EDGE_CURVE('',#3107,#3106,#1867,.T.);
#3850=EDGE_CURVE('',#3110,#3110,#2636,.T.);
#3851=EDGE_CURVE('',#3110,#3111,#1868,.T.);
#3852=EDGE_CURVE('',#3111,#3111,#2637,.F.);
#3853=EDGE_CURVE('',#3112,#3113,#1869,.T.);
#3854=EDGE_CURVE('',#3113,#3114,#1870,.T.);
#3855=EDGE_CURVE('',#3114,#3115,#2638,.F.);
#3856=EDGE_CURVE('',#3115,#3112,#1871,.T.);
#3857=EDGE_CURVE('',#3116,#3116,#2639,.T.);
#3858=EDGE_CURVE('',#3116,#3117,#1872,.T.);
#3859=EDGE_CURVE('',#3117,#3117,#2640,.F.);
#3860=EDGE_CURVE('',#3118,#3115,#1873,.T.);
#3861=EDGE_CURVE('',#3119,#3118,#1874,.T.);
#3862=EDGE_CURVE('',#3112,#3119,#1875,.T.);
#3863=EDGE_CURVE('',#3114,#3120,#1876,.F.);
#3864=EDGE_CURVE('',#3120,#3118,#2641,.F.);
#3865=EDGE_CURVE('',#3121,#3113,#1877,.T.);
#3866=EDGE_CURVE('',#3120,#3121,#1878,.T.);
#3867=EDGE_CURVE('',#3121,#3119,#1879,.T.);
#3868=EDGE_CURVE('',#3122,#3122,#2642,.T.);
#3869=EDGE_CURVE('',#3122,#3123,#1880,.T.);
#3870=EDGE_CURVE('',#3123,#3123,#2643,.F.);
#3871=EDGE_CURVE('',#3124,#3125,#1881,.T.);
#3872=EDGE_CURVE('',#3125,#3126,#1882,.T.);
#3873=EDGE_CURVE('',#3126,#3127,#2644,.F.);
#3874=EDGE_CURVE('',#3127,#3124,#1883,.T.);
#3875=EDGE_CURVE('',#3128,#3128,#2645,.T.);
#3876=EDGE_CURVE('',#3128,#3129,#1884,.T.);
#3877=EDGE_CURVE('',#3129,#3129,#2646,.F.);
#3878=EDGE_CURVE('',#3130,#3127,#1885,.T.);
#3879=EDGE_CURVE('',#3131,#3130,#1886,.T.);
#3880=EDGE_CURVE('',#3124,#3131,#1887,.T.);
#3881=EDGE_CURVE('',#3126,#3132,#1888,.F.);
#3882=EDGE_CURVE('',#3132,#3130,#2647,.F.);
#3883=EDGE_CURVE('',#3133,#3125,#1889,.T.);
#3884=EDGE_CURVE('',#3132,#3133,#1890,.T.);
#3885=EDGE_CURVE('',#3133,#3131,#1891,.T.);
#3886=EDGE_CURVE('',#3134,#3135,#11,.T.);
#3887=EDGE_CURVE('',#3135,#3134,#12,.F.);
#3888=EDGE_CURVE('',#3135,#3136,#1892,.T.);
#3889=EDGE_CURVE('',#3136,#3137,#13,.F.);
#3890=EDGE_CURVE('',#3137,#3136,#14,.T.);
#3891=EDGE_CURVE('',#3138,#3138,#2648,.F.);
#3892=EDGE_CURVE('',#3138,#3139,#1893,.T.);
#3893=EDGE_CURVE('',#3139,#3139,#2649,.T.);
#3894=EDGE_CURVE('',#3140,#3140,#2650,.T.);
#3895=EDGE_CURVE('',#3140,#3141,#1894,.T.);
#3896=EDGE_CURVE('',#3141,#3141,#2651,.F.);
#3897=EDGE_CURVE('',#3142,#3142,#2652,.F.);
#3898=EDGE_CURVE('',#3143,#3143,#2653,.F.);
#3899=EDGE_CURVE('',#3142,#3143,#1895,.T.);
#3900=EDGE_CURVE('',#3144,#3145,#15,.T.);
#3901=EDGE_CURVE('',#3145,#3144,#16,.F.);
#3902=EDGE_CURVE('',#3144,#3146,#1896,.T.);
#3903=EDGE_CURVE('',#3146,#3147,#17,.T.);
#3904=EDGE_CURVE('',#3147,#3146,#18,.F.);
#3905=EDGE_CURVE('',#3148,#3148,#2654,.F.);
#3906=EDGE_CURVE('',#3148,#3149,#1897,.T.);
#3907=EDGE_CURVE('',#3149,#3149,#2655,.T.);
#3908=EDGE_CURVE('',#3150,#3150,#2656,.F.);
#3909=EDGE_CURVE('',#3150,#3151,#1898,.T.);
#3910=EDGE_CURVE('',#3151,#3151,#2657,.T.);
#3911=EDGE_CURVE('',#3152,#3152,#2658,.F.);
#3912=EDGE_CURVE('',#3153,#3154,#1899,.T.);
#3913=EDGE_CURVE('',#3155,#3153,#1900,.T.);
#3914=EDGE_CURVE('',#3156,#3155,#2659,.T.);
#3915=EDGE_CURVE('',#3154,#3156,#2660,.F.);
#3916=EDGE_CURVE('',#3157,#3157,#2661,.T.);
#3917=EDGE_CURVE('',#3158,#3158,#2662,.T.);
#3918=EDGE_CURVE('',#3159,#3159,#2663,.T.);
#3919=EDGE_CURVE('',#3160,#3160,#2664,.T.);
#3920=EDGE_CURVE('',#3161,#3161,#2665,.T.);
#3921=EDGE_CURVE('',#3161,#3152,#1901,.T.);
#3922=EDGE_CURVE('',#3162,#3162,#2666,.T.);
#3923=EDGE_CURVE('',#3162,#3160,#1902,.T.);
#3924=EDGE_CURVE('',#3163,#3163,#2667,.T.);
#3925=EDGE_CURVE('',#3163,#3159,#1903,.T.);
#3926=EDGE_CURVE('',#3164,#3164,#2668,.T.);
#3927=EDGE_CURVE('',#3164,#3158,#1904,.T.);
#3928=EDGE_CURVE('',#3165,#3165,#2669,.T.);
#3929=EDGE_CURVE('',#3165,#3157,#1905,.T.);
#3930=EDGE_CURVE('',#3155,#3166,#1906,.T.);
#3931=EDGE_CURVE('',#3167,#3153,#1907,.T.);
#3932=EDGE_CURVE('',#3166,#3167,#1908,.T.);
#3933=EDGE_CURVE('',#3168,#3166,#2670,.T.);
#3934=EDGE_CURVE('',#3156,#3168,#1909,.F.);
#3935=EDGE_CURVE('',#3169,#3154,#1910,.F.);
#3936=EDGE_CURVE('',#3168,#3169,#2671,.T.);
#3937=EDGE_CURVE('',#3169,#3167,#1911,.T.);
#3938=EDGE_CURVE('',#3170,#3170,#2672,.T.);
#3939=EDGE_CURVE('',#3170,#3171,#1912,.T.);
#3940=EDGE_CURVE('',#3171,#3171,#2673,.F.);
#3941=EDGE_CURVE('',#3172,#3172,#2674,.F.);
#3942=EDGE_CURVE('',#3173,#3173,#2675,.F.);
#3943=EDGE_CURVE('',#3172,#3173,#1913,.T.);
#3944=EDGE_CURVE('',#3174,#3174,#2676,.T.);
#3945=EDGE_CURVE('',#3174,#3175,#1914,.T.);
#3946=EDGE_CURVE('',#3175,#3175,#2677,.F.);
#3947=EDGE_CURVE('',#3176,#3176,#2678,.F.);
#3948=EDGE_CURVE('',#3177,#3177,#2679,.F.);
#3949=EDGE_CURVE('',#3176,#3177,#1915,.T.);
#3950=EDGE_CURVE('',#3178,#3178,#2680,.F.);
#3951=EDGE_CURVE('',#3178,#3179,#1916,.T.);
#3952=EDGE_CURVE('',#3179,#3179,#2681,.T.);
#3953=ORIENTED_EDGE('',*,*,#3180,.T.);
#3954=ORIENTED_EDGE('',*,*,#3181,.T.);
#3955=ORIENTED_EDGE('',*,*,#3182,.F.);
#3956=ORIENTED_EDGE('',*,*,#3181,.F.);
#3957=ORIENTED_EDGE('',*,*,#3183,.T.);
#3958=ORIENTED_EDGE('',*,*,#3184,.T.);
#3959=ORIENTED_EDGE('',*,*,#3185,.T.);
#3960=ORIENTED_EDGE('',*,*,#3186,.T.);
#3961=ORIENTED_EDGE('',*,*,#3184,.F.);
#3962=ORIENTED_EDGE('',*,*,#3187,.T.);
#3963=ORIENTED_EDGE('',*,*,#3188,.T.);
#3964=ORIENTED_EDGE('',*,*,#3185,.F.);
#3965=ORIENTED_EDGE('',*,*,#3186,.F.);
#3966=ORIENTED_EDGE('',*,*,#3188,.F.);
#3967=ORIENTED_EDGE('',*,*,#3189,.T.);
#3968=ORIENTED_EDGE('',*,*,#3190,.T.);
#3969=ORIENTED_EDGE('',*,*,#3183,.F.);
#3970=ORIENTED_EDGE('',*,*,#3190,.F.);
#3971=ORIENTED_EDGE('',*,*,#3191,.T.);
#3972=ORIENTED_EDGE('',*,*,#3192,.T.);
#3973=ORIENTED_EDGE('',*,*,#3193,.T.);
#3974=ORIENTED_EDGE('',*,*,#3187,.F.);
#3975=ORIENTED_EDGE('',*,*,#3193,.F.);
#3976=ORIENTED_EDGE('',*,*,#3189,.F.);
#3977=ORIENTED_EDGE('',*,*,#3194,.T.);
#3978=ORIENTED_EDGE('',*,*,#3195,.T.);
#3979=ORIENTED_EDGE('',*,*,#3194,.F.);
#3980=ORIENTED_EDGE('',*,*,#3191,.F.);
#3981=ORIENTED_EDGE('',*,*,#3192,.F.);
#3982=ORIENTED_EDGE('',*,*,#3196,.F.);
#3983=ORIENTED_EDGE('',*,*,#3195,.F.);
#3984=ORIENTED_EDGE('',*,*,#3197,.T.);
#3985=ORIENTED_EDGE('',*,*,#3198,.F.);
#3986=ORIENTED_EDGE('',*,*,#3199,.T.);
#3987=ORIENTED_EDGE('',*,*,#3196,.T.);
#3988=ORIENTED_EDGE('',*,*,#3199,.F.);
#3989=ORIENTED_EDGE('',*,*,#3197,.F.);
#3990=ORIENTED_EDGE('',*,*,#3200,.T.);
#3991=ORIENTED_EDGE('',*,*,#3201,.F.);
#3992=ORIENTED_EDGE('',*,*,#3200,.F.);
#3993=ORIENTED_EDGE('',*,*,#3198,.T.);
#3994=ORIENTED_EDGE('',*,*,#3202,.F.);
#3995=ORIENTED_EDGE('',*,*,#3203,.F.);
#3996=ORIENTED_EDGE('',*,*,#3204,.F.);
#3997=ORIENTED_EDGE('',*,*,#3205,.F.);
#3998=ORIENTED_EDGE('',*,*,#3206,.F.);
#3999=ORIENTED_EDGE('',*,*,#3207,.F.);
#4000=ORIENTED_EDGE('',*,*,#3208,.F.);
#4001=ORIENTED_EDGE('',*,*,#3201,.T.);
#4002=ORIENTED_EDGE('',*,*,#3209,.T.);
#4003=ORIENTED_EDGE('',*,*,#3210,.T.);
#4004=ORIENTED_EDGE('',*,*,#3211,.T.);
#4005=ORIENTED_EDGE('',*,*,#3212,.T.);
#4006=ORIENTED_EDGE('',*,*,#3213,.T.);
#4007=ORIENTED_EDGE('',*,*,#3214,.T.);
#4008=ORIENTED_EDGE('',*,*,#3215,.T.);
#4009=ORIENTED_EDGE('',*,*,#3216,.T.);
#4010=ORIENTED_EDGE('',*,*,#3217,.T.);
#4011=ORIENTED_EDGE('',*,*,#3208,.T.);
#4012=ORIENTED_EDGE('',*,*,#3217,.F.);
#4013=ORIENTED_EDGE('',*,*,#3207,.T.);
#4014=ORIENTED_EDGE('',*,*,#3218,.T.);
#4015=ORIENTED_EDGE('',*,*,#3214,.F.);
#4016=ORIENTED_EDGE('',*,*,#3218,.F.);
#4017=ORIENTED_EDGE('',*,*,#3206,.T.);
#4018=ORIENTED_EDGE('',*,*,#3219,.T.);
#4019=ORIENTED_EDGE('',*,*,#3213,.F.);
#4020=ORIENTED_EDGE('',*,*,#3219,.F.);
#4021=ORIENTED_EDGE('',*,*,#3205,.T.);
#4022=ORIENTED_EDGE('',*,*,#3220,.T.);
#4023=ORIENTED_EDGE('',*,*,#3212,.F.);
#4024=ORIENTED_EDGE('',*,*,#3220,.F.);
#4025=ORIENTED_EDGE('',*,*,#3204,.T.);
#4026=ORIENTED_EDGE('',*,*,#3221,.T.);
#4027=ORIENTED_EDGE('',*,*,#3211,.F.);
#4028=ORIENTED_EDGE('',*,*,#3221,.F.);
#4029=ORIENTED_EDGE('',*,*,#3203,.T.);
#4030=ORIENTED_EDGE('',*,*,#3222,.T.);
#4031=ORIENTED_EDGE('',*,*,#3210,.F.);
#4032=ORIENTED_EDGE('',*,*,#3222,.F.);
#4033=ORIENTED_EDGE('',*,*,#3202,.T.);
#4034=ORIENTED_EDGE('',*,*,#3223,.T.);
#4035=ORIENTED_EDGE('',*,*,#3209,.F.);
#4036=ORIENTED_EDGE('',*,*,#3223,.F.);
#4037=ORIENTED_EDGE('',*,*,#3215,.F.);
#4038=ORIENTED_EDGE('',*,*,#3224,.T.);
#4039=ORIENTED_EDGE('',*,*,#3225,.T.);
#4040=ORIENTED_EDGE('',*,*,#3224,.F.);
#4041=ORIENTED_EDGE('',*,*,#3216,.F.);
#4042=ORIENTED_EDGE('',*,*,#3182,.T.);
#4043=ORIENTED_EDGE('',*,*,#3225,.F.);
#4044=ORIENTED_EDGE('',*,*,#3180,.F.);
#4045=ORIENTED_EDGE('',*,*,#3226,.T.);
#4046=ORIENTED_EDGE('',*,*,#3227,.T.);
#4047=ORIENTED_EDGE('',*,*,#3228,.T.);
#4048=ORIENTED_EDGE('',*,*,#3229,.T.);
#4049=ORIENTED_EDGE('',*,*,#3227,.F.);
#4050=ORIENTED_EDGE('',*,*,#3230,.T.);
#4051=ORIENTED_EDGE('',*,*,#3229,.F.);
#4052=ORIENTED_EDGE('',*,*,#3231,.T.);
#4053=ORIENTED_EDGE('',*,*,#3232,.T.);
#4054=ORIENTED_EDGE('',*,*,#3233,.T.);
#4055=ORIENTED_EDGE('',*,*,#3234,.T.);
#4056=ORIENTED_EDGE('',*,*,#3231,.F.);
#4057=ORIENTED_EDGE('',*,*,#3228,.F.);
#4058=ORIENTED_EDGE('',*,*,#3234,.F.);
#4059=ORIENTED_EDGE('',*,*,#3226,.F.);
#4060=ORIENTED_EDGE('',*,*,#3230,.F.);
#4061=ORIENTED_EDGE('',*,*,#3235,.T.);
#4062=ORIENTED_EDGE('',*,*,#3232,.F.);
#4063=ORIENTED_EDGE('',*,*,#3236,.T.);
#4064=ORIENTED_EDGE('',*,*,#3237,.T.);
#4065=ORIENTED_EDGE('',*,*,#3238,.T.);
#4066=ORIENTED_EDGE('',*,*,#3235,.F.);
#4067=ORIENTED_EDGE('',*,*,#3239,.T.);
#4068=ORIENTED_EDGE('',*,*,#3240,.F.);
#4069=ORIENTED_EDGE('',*,*,#3241,.F.);
#4070=ORIENTED_EDGE('',*,*,#3239,.F.);
#4071=ORIENTED_EDGE('',*,*,#3236,.F.);
#4072=ORIENTED_EDGE('',*,*,#3233,.F.);
#4073=ORIENTED_EDGE('',*,*,#3238,.F.);
#4074=ORIENTED_EDGE('',*,*,#3242,.T.);
#4075=ORIENTED_EDGE('',*,*,#3237,.F.);
#4076=ORIENTED_EDGE('',*,*,#3242,.F.);
#4077=ORIENTED_EDGE('',*,*,#3243,.T.);
#4078=ORIENTED_EDGE('',*,*,#3241,.T.);
#4079=ORIENTED_EDGE('',*,*,#3244,.T.);
#4080=ORIENTED_EDGE('',*,*,#3245,.T.);
#4081=ORIENTED_EDGE('',*,*,#3246,.T.);
#4082=ORIENTED_EDGE('',*,*,#3244,.F.);
#4083=ORIENTED_EDGE('',*,*,#3240,.T.);
#4084=ORIENTED_EDGE('',*,*,#3247,.F.);
#4085=ORIENTED_EDGE('',*,*,#3248,.F.);
#4086=ORIENTED_EDGE('',*,*,#3249,.T.);
#4087=ORIENTED_EDGE('',*,*,#3243,.F.);
#4088=ORIENTED_EDGE('',*,*,#3249,.F.);
#4089=ORIENTED_EDGE('',*,*,#3246,.F.);
#4090=ORIENTED_EDGE('',*,*,#3250,.T.);
#4091=ORIENTED_EDGE('',*,*,#3251,.T.);
#4092=ORIENTED_EDGE('',*,*,#3250,.F.);
#4093=ORIENTED_EDGE('',*,*,#3245,.F.);
#4094=ORIENTED_EDGE('',*,*,#3252,.T.);
#4095=ORIENTED_EDGE('',*,*,#3253,.T.);
#4096=ORIENTED_EDGE('',*,*,#3247,.T.);
#4097=ORIENTED_EDGE('',*,*,#3248,.T.);
#4098=ORIENTED_EDGE('',*,*,#3253,.F.);
#4099=ORIENTED_EDGE('',*,*,#3254,.T.);
#4100=ORIENTED_EDGE('',*,*,#3251,.F.);
#4101=ORIENTED_EDGE('',*,*,#3255,.T.);
#4102=ORIENTED_EDGE('',*,*,#3256,.T.);
#4103=ORIENTED_EDGE('',*,*,#3257,.T.);
#4104=ORIENTED_EDGE('',*,*,#3258,.T.);
#4105=ORIENTED_EDGE('',*,*,#3254,.F.);
#4106=ORIENTED_EDGE('',*,*,#3252,.F.);
#4107=ORIENTED_EDGE('',*,*,#3258,.F.);
#4108=ORIENTED_EDGE('',*,*,#3259,.T.);
#4109=ORIENTED_EDGE('',*,*,#3260,.T.);
#4110=ORIENTED_EDGE('',*,*,#3261,.T.);
#4111=ORIENTED_EDGE('',*,*,#3256,.F.);
#4112=ORIENTED_EDGE('',*,*,#3262,.T.);
#4113=ORIENTED_EDGE('',*,*,#3259,.F.);
#4114=ORIENTED_EDGE('',*,*,#3255,.F.);
#4115=ORIENTED_EDGE('',*,*,#3261,.F.);
#4116=ORIENTED_EDGE('',*,*,#3257,.F.);
#4117=ORIENTED_EDGE('',*,*,#3263,.T.);
#4118=ORIENTED_EDGE('',*,*,#3264,.T.);
#4119=ORIENTED_EDGE('',*,*,#3260,.F.);
#4120=ORIENTED_EDGE('',*,*,#3265,.T.);
#4121=ORIENTED_EDGE('',*,*,#3266,.F.);
#4122=ORIENTED_EDGE('',*,*,#3267,.F.);
#4123=ORIENTED_EDGE('',*,*,#3265,.F.);
#4124=ORIENTED_EDGE('',*,*,#3262,.F.);
#4125=ORIENTED_EDGE('',*,*,#3268,.T.);
#4126=ORIENTED_EDGE('',*,*,#3264,.F.);
#4127=ORIENTED_EDGE('',*,*,#3269,.T.);
#4128=ORIENTED_EDGE('',*,*,#3266,.T.);
#4129=ORIENTED_EDGE('',*,*,#3263,.F.);
#4130=ORIENTED_EDGE('',*,*,#3268,.F.);
#4131=ORIENTED_EDGE('',*,*,#3267,.T.);
#4132=ORIENTED_EDGE('',*,*,#3269,.F.);
#4133=ORIENTED_EDGE('',*,*,#3270,.T.);
#4134=ORIENTED_EDGE('',*,*,#3271,.T.);
#4135=ORIENTED_EDGE('',*,*,#3272,.T.);
#4136=ORIENTED_EDGE('',*,*,#3273,.T.);
#4137=ORIENTED_EDGE('',*,*,#3271,.F.);
#4138=ORIENTED_EDGE('',*,*,#3274,.T.);
#4139=ORIENTED_EDGE('',*,*,#3273,.F.);
#4140=ORIENTED_EDGE('',*,*,#3275,.T.);
#4141=ORIENTED_EDGE('',*,*,#3276,.T.);
#4142=ORIENTED_EDGE('',*,*,#3277,.T.);
#4143=ORIENTED_EDGE('',*,*,#3278,.T.);
#4144=ORIENTED_EDGE('',*,*,#3275,.F.);
#4145=ORIENTED_EDGE('',*,*,#3272,.F.);
#4146=ORIENTED_EDGE('',*,*,#3278,.F.);
#4147=ORIENTED_EDGE('',*,*,#3270,.F.);
#4148=ORIENTED_EDGE('',*,*,#3274,.F.);
#4149=ORIENTED_EDGE('',*,*,#3279,.T.);
#4150=ORIENTED_EDGE('',*,*,#3276,.F.);
#4151=ORIENTED_EDGE('',*,*,#3280,.T.);
#4152=ORIENTED_EDGE('',*,*,#3281,.T.);
#4153=ORIENTED_EDGE('',*,*,#3282,.T.);
#4154=ORIENTED_EDGE('',*,*,#3279,.F.);
#4155=ORIENTED_EDGE('',*,*,#3283,.T.);
#4156=ORIENTED_EDGE('',*,*,#3284,.F.);
#4157=ORIENTED_EDGE('',*,*,#3285,.F.);
#4158=ORIENTED_EDGE('',*,*,#3283,.F.);
#4159=ORIENTED_EDGE('',*,*,#3280,.F.);
#4160=ORIENTED_EDGE('',*,*,#3277,.F.);
#4161=ORIENTED_EDGE('',*,*,#3282,.F.);
#4162=ORIENTED_EDGE('',*,*,#3286,.T.);
#4163=ORIENTED_EDGE('',*,*,#3281,.F.);
#4164=ORIENTED_EDGE('',*,*,#3286,.F.);
#4165=ORIENTED_EDGE('',*,*,#3287,.T.);
#4166=ORIENTED_EDGE('',*,*,#3285,.T.);
#4167=ORIENTED_EDGE('',*,*,#3288,.T.);
#4168=ORIENTED_EDGE('',*,*,#3289,.T.);
#4169=ORIENTED_EDGE('',*,*,#3290,.T.);
#4170=ORIENTED_EDGE('',*,*,#3288,.F.);
#4171=ORIENTED_EDGE('',*,*,#3284,.T.);
#4172=ORIENTED_EDGE('',*,*,#3291,.F.);
#4173=ORIENTED_EDGE('',*,*,#3292,.F.);
#4174=ORIENTED_EDGE('',*,*,#3293,.T.);
#4175=ORIENTED_EDGE('',*,*,#3287,.F.);
#4176=ORIENTED_EDGE('',*,*,#3293,.F.);
#4177=ORIENTED_EDGE('',*,*,#3290,.F.);
#4178=ORIENTED_EDGE('',*,*,#3294,.T.);
#4179=ORIENTED_EDGE('',*,*,#3295,.T.);
#4180=ORIENTED_EDGE('',*,*,#3294,.F.);
#4181=ORIENTED_EDGE('',*,*,#3289,.F.);
#4182=ORIENTED_EDGE('',*,*,#3296,.T.);
#4183=ORIENTED_EDGE('',*,*,#3297,.T.);
#4184=ORIENTED_EDGE('',*,*,#3291,.T.);
#4185=ORIENTED_EDGE('',*,*,#3292,.T.);
#4186=ORIENTED_EDGE('',*,*,#3297,.F.);
#4187=ORIENTED_EDGE('',*,*,#3298,.T.);
#4188=ORIENTED_EDGE('',*,*,#3295,.F.);
#4189=ORIENTED_EDGE('',*,*,#3299,.T.);
#4190=ORIENTED_EDGE('',*,*,#3300,.T.);
#4191=ORIENTED_EDGE('',*,*,#3301,.T.);
#4192=ORIENTED_EDGE('',*,*,#3302,.T.);
#4193=ORIENTED_EDGE('',*,*,#3298,.F.);
#4194=ORIENTED_EDGE('',*,*,#3296,.F.);
#4195=ORIENTED_EDGE('',*,*,#3302,.F.);
#4196=ORIENTED_EDGE('',*,*,#3303,.T.);
#4197=ORIENTED_EDGE('',*,*,#3304,.T.);
#4198=ORIENTED_EDGE('',*,*,#3305,.T.);
#4199=ORIENTED_EDGE('',*,*,#3300,.F.);
#4200=ORIENTED_EDGE('',*,*,#3306,.T.);
#4201=ORIENTED_EDGE('',*,*,#3303,.F.);
#4202=ORIENTED_EDGE('',*,*,#3299,.F.);
#4203=ORIENTED_EDGE('',*,*,#3305,.F.);
#4204=ORIENTED_EDGE('',*,*,#3301,.F.);
#4205=ORIENTED_EDGE('',*,*,#3307,.T.);
#4206=ORIENTED_EDGE('',*,*,#3308,.T.);
#4207=ORIENTED_EDGE('',*,*,#3304,.F.);
#4208=ORIENTED_EDGE('',*,*,#3309,.T.);
#4209=ORIENTED_EDGE('',*,*,#3310,.F.);
#4210=ORIENTED_EDGE('',*,*,#3311,.F.);
#4211=ORIENTED_EDGE('',*,*,#3309,.F.);
#4212=ORIENTED_EDGE('',*,*,#3306,.F.);
#4213=ORIENTED_EDGE('',*,*,#3312,.T.);
#4214=ORIENTED_EDGE('',*,*,#3308,.F.);
#4215=ORIENTED_EDGE('',*,*,#3313,.T.);
#4216=ORIENTED_EDGE('',*,*,#3310,.T.);
#4217=ORIENTED_EDGE('',*,*,#3307,.F.);
#4218=ORIENTED_EDGE('',*,*,#3312,.F.);
#4219=ORIENTED_EDGE('',*,*,#3311,.T.);
#4220=ORIENTED_EDGE('',*,*,#3313,.F.);
#4221=ORIENTED_EDGE('',*,*,#3314,.T.);
#4222=ORIENTED_EDGE('',*,*,#3315,.T.);
#4223=ORIENTED_EDGE('',*,*,#3316,.T.);
#4224=ORIENTED_EDGE('',*,*,#3317,.T.);
#4225=ORIENTED_EDGE('',*,*,#3315,.F.);
#4226=ORIENTED_EDGE('',*,*,#3318,.T.);
#4227=ORIENTED_EDGE('',*,*,#3319,.T.);
#4228=ORIENTED_EDGE('',*,*,#3316,.F.);
#4229=ORIENTED_EDGE('',*,*,#3317,.F.);
#4230=ORIENTED_EDGE('',*,*,#3319,.F.);
#4231=ORIENTED_EDGE('',*,*,#3320,.T.);
#4232=ORIENTED_EDGE('',*,*,#3321,.T.);
#4233=ORIENTED_EDGE('',*,*,#3314,.F.);
#4234=ORIENTED_EDGE('',*,*,#3321,.F.);
#4235=ORIENTED_EDGE('',*,*,#3322,.T.);
#4236=ORIENTED_EDGE('',*,*,#3323,.T.);
#4237=ORIENTED_EDGE('',*,*,#3324,.T.);
#4238=ORIENTED_EDGE('',*,*,#3318,.F.);
#4239=ORIENTED_EDGE('',*,*,#3324,.F.);
#4240=ORIENTED_EDGE('',*,*,#3320,.F.);
#4241=ORIENTED_EDGE('',*,*,#3325,.T.);
#4242=ORIENTED_EDGE('',*,*,#3326,.T.);
#4243=ORIENTED_EDGE('',*,*,#3325,.F.);
#4244=ORIENTED_EDGE('',*,*,#3322,.F.);
#4245=ORIENTED_EDGE('',*,*,#3323,.F.);
#4246=ORIENTED_EDGE('',*,*,#3327,.F.);
#4247=ORIENTED_EDGE('',*,*,#3326,.F.);
#4248=ORIENTED_EDGE('',*,*,#3328,.T.);
#4249=ORIENTED_EDGE('',*,*,#3329,.F.);
#4250=ORIENTED_EDGE('',*,*,#3330,.T.);
#4251=ORIENTED_EDGE('',*,*,#3327,.T.);
#4252=ORIENTED_EDGE('',*,*,#3330,.F.);
#4253=ORIENTED_EDGE('',*,*,#3328,.F.);
#4254=ORIENTED_EDGE('',*,*,#3331,.T.);
#4255=ORIENTED_EDGE('',*,*,#3332,.F.);
#4256=ORIENTED_EDGE('',*,*,#3331,.F.);
#4257=ORIENTED_EDGE('',*,*,#3329,.T.);
#4258=ORIENTED_EDGE('',*,*,#3333,.F.);
#4259=ORIENTED_EDGE('',*,*,#3334,.F.);
#4260=ORIENTED_EDGE('',*,*,#3335,.F.);
#4261=ORIENTED_EDGE('',*,*,#3336,.F.);
#4262=ORIENTED_EDGE('',*,*,#3337,.F.);
#4263=ORIENTED_EDGE('',*,*,#3338,.F.);
#4264=ORIENTED_EDGE('',*,*,#3339,.F.);
#4265=ORIENTED_EDGE('',*,*,#3332,.T.);
#4266=ORIENTED_EDGE('',*,*,#3340,.T.);
#4267=ORIENTED_EDGE('',*,*,#3341,.T.);
#4268=ORIENTED_EDGE('',*,*,#3342,.T.);
#4269=ORIENTED_EDGE('',*,*,#3343,.T.);
#4270=ORIENTED_EDGE('',*,*,#3344,.T.);
#4271=ORIENTED_EDGE('',*,*,#3345,.T.);
#4272=ORIENTED_EDGE('',*,*,#3346,.T.);
#4273=ORIENTED_EDGE('',*,*,#3347,.T.);
#4274=ORIENTED_EDGE('',*,*,#3348,.T.);
#4275=ORIENTED_EDGE('',*,*,#3339,.T.);
#4276=ORIENTED_EDGE('',*,*,#3348,.F.);
#4277=ORIENTED_EDGE('',*,*,#3338,.T.);
#4278=ORIENTED_EDGE('',*,*,#3349,.T.);
#4279=ORIENTED_EDGE('',*,*,#3345,.F.);
#4280=ORIENTED_EDGE('',*,*,#3349,.F.);
#4281=ORIENTED_EDGE('',*,*,#3337,.T.);
#4282=ORIENTED_EDGE('',*,*,#3350,.T.);
#4283=ORIENTED_EDGE('',*,*,#3344,.F.);
#4284=ORIENTED_EDGE('',*,*,#3350,.F.);
#4285=ORIENTED_EDGE('',*,*,#3336,.T.);
#4286=ORIENTED_EDGE('',*,*,#3351,.T.);
#4287=ORIENTED_EDGE('',*,*,#3343,.F.);
#4288=ORIENTED_EDGE('',*,*,#3351,.F.);
#4289=ORIENTED_EDGE('',*,*,#3335,.T.);
#4290=ORIENTED_EDGE('',*,*,#3352,.T.);
#4291=ORIENTED_EDGE('',*,*,#3342,.F.);
#4292=ORIENTED_EDGE('',*,*,#3352,.F.);
#4293=ORIENTED_EDGE('',*,*,#3334,.T.);
#4294=ORIENTED_EDGE('',*,*,#3353,.T.);
#4295=ORIENTED_EDGE('',*,*,#3341,.F.);
#4296=ORIENTED_EDGE('',*,*,#3353,.F.);
#4297=ORIENTED_EDGE('',*,*,#3333,.T.);
#4298=ORIENTED_EDGE('',*,*,#3354,.T.);
#4299=ORIENTED_EDGE('',*,*,#3340,.F.);
#4300=ORIENTED_EDGE('',*,*,#3354,.F.);
#4301=ORIENTED_EDGE('',*,*,#3346,.F.);
#4302=ORIENTED_EDGE('',*,*,#3355,.T.);
#4303=ORIENTED_EDGE('',*,*,#3356,.T.);
#4304=ORIENTED_EDGE('',*,*,#3355,.F.);
#4305=ORIENTED_EDGE('',*,*,#3347,.F.);
#4306=ORIENTED_EDGE('',*,*,#3357,.F.);
#4307=ORIENTED_EDGE('',*,*,#3356,.F.);
#4308=ORIENTED_EDGE('',*,*,#3358,.T.);
#4309=ORIENTED_EDGE('',*,*,#3358,.F.);
#4310=ORIENTED_EDGE('',*,*,#3359,.T.);
#4311=ORIENTED_EDGE('',*,*,#3357,.T.);
#4312=ORIENTED_EDGE('',*,*,#3359,.F.);
#4313=ORIENTED_EDGE('',*,*,#3360,.F.);
#4314=ORIENTED_EDGE('',*,*,#3361,.F.);
#4315=ORIENTED_EDGE('',*,*,#3362,.F.);
#4316=ORIENTED_EDGE('',*,*,#3363,.F.);
#4317=ORIENTED_EDGE('',*,*,#3363,.T.);
#4318=ORIENTED_EDGE('',*,*,#3364,.F.);
#4319=ORIENTED_EDGE('',*,*,#3365,.F.);
#4320=ORIENTED_EDGE('',*,*,#3366,.F.);
#4321=ORIENTED_EDGE('',*,*,#3362,.T.);
#4322=ORIENTED_EDGE('',*,*,#3367,.F.);
#4323=ORIENTED_EDGE('',*,*,#3368,.F.);
#4324=ORIENTED_EDGE('',*,*,#3369,.F.);
#4325=ORIENTED_EDGE('',*,*,#3370,.F.);
#4326=ORIENTED_EDGE('',*,*,#3371,.F.);
#4327=ORIENTED_EDGE('',*,*,#3360,.T.);
#4328=ORIENTED_EDGE('',*,*,#3372,.F.);
#4329=ORIENTED_EDGE('',*,*,#3369,.T.);
#4330=ORIENTED_EDGE('',*,*,#3373,.F.);
#4331=ORIENTED_EDGE('',*,*,#3374,.F.);
#4332=ORIENTED_EDGE('',*,*,#3364,.T.);
#4333=ORIENTED_EDGE('',*,*,#3375,.F.);
#4334=ORIENTED_EDGE('',*,*,#3376,.F.);
#4335=ORIENTED_EDGE('',*,*,#3365,.T.);
#4336=ORIENTED_EDGE('',*,*,#3377,.F.);
#4337=ORIENTED_EDGE('',*,*,#3378,.F.);
#4338=ORIENTED_EDGE('',*,*,#3372,.T.);
#4339=ORIENTED_EDGE('',*,*,#3366,.T.);
#4340=ORIENTED_EDGE('',*,*,#3379,.F.);
#4341=ORIENTED_EDGE('',*,*,#3368,.T.);
#4342=ORIENTED_EDGE('',*,*,#3380,.T.);
#4343=ORIENTED_EDGE('',*,*,#3370,.T.);
#4344=ORIENTED_EDGE('',*,*,#3381,.T.);
#4345=ORIENTED_EDGE('',*,*,#3382,.F.);
#4346=ORIENTED_EDGE('',*,*,#3361,.T.);
#4347=ORIENTED_EDGE('',*,*,#3383,.F.);
#4348=ORIENTED_EDGE('',*,*,#3375,.T.);
#4349=ORIENTED_EDGE('',*,*,#3371,.T.);
#4350=ORIENTED_EDGE('',*,*,#3384,.F.);
#4351=ORIENTED_EDGE('',*,*,#3385,.F.);
#4352=ORIENTED_EDGE('',*,*,#3383,.T.);
#4353=ORIENTED_EDGE('',*,*,#3381,.F.);
#4354=ORIENTED_EDGE('',*,*,#3378,.T.);
#4355=ORIENTED_EDGE('',*,*,#3386,.F.);
#4356=ORIENTED_EDGE('',*,*,#3373,.T.);
#4357=ORIENTED_EDGE('',*,*,#3377,.T.);
#4358=ORIENTED_EDGE('',*,*,#3374,.T.);
#4359=ORIENTED_EDGE('',*,*,#3387,.F.);
#4360=ORIENTED_EDGE('',*,*,#3388,.F.);
#4361=ORIENTED_EDGE('',*,*,#3376,.T.);
#4362=ORIENTED_EDGE('',*,*,#3385,.T.);
#4363=ORIENTED_EDGE('',*,*,#3389,.F.);
#4364=ORIENTED_EDGE('',*,*,#3379,.T.);
#4365=ORIENTED_EDGE('',*,*,#3367,.T.);
#4366=ORIENTED_EDGE('',*,*,#3382,.T.);
#4367=ORIENTED_EDGE('',*,*,#3388,.T.);
#4368=ORIENTED_EDGE('',*,*,#3390,.F.);
#4369=ORIENTED_EDGE('',*,*,#3380,.F.);
#4370=ORIENTED_EDGE('',*,*,#3390,.T.);
#4371=ORIENTED_EDGE('',*,*,#3391,.F.);
#4372=ORIENTED_EDGE('',*,*,#3384,.T.);
#4373=ORIENTED_EDGE('',*,*,#3391,.T.);
#4374=ORIENTED_EDGE('',*,*,#3387,.T.);
#4375=ORIENTED_EDGE('',*,*,#3386,.T.);
#4376=ORIENTED_EDGE('',*,*,#3389,.T.);
#4377=ORIENTED_EDGE('',*,*,#3392,.F.);
#4378=ORIENTED_EDGE('',*,*,#3393,.T.);
#4379=ORIENTED_EDGE('',*,*,#3394,.F.);
#4380=ORIENTED_EDGE('',*,*,#3393,.F.);
#4381=ORIENTED_EDGE('',*,*,#3395,.F.);
#4382=ORIENTED_EDGE('',*,*,#3396,.F.);
#4383=ORIENTED_EDGE('',*,*,#3397,.F.);
#4384=ORIENTED_EDGE('',*,*,#3398,.F.);
#4385=ORIENTED_EDGE('',*,*,#3394,.T.);
#4386=ORIENTED_EDGE('',*,*,#3399,.F.);
#4387=ORIENTED_EDGE('',*,*,#3400,.F.);
#4388=ORIENTED_EDGE('',*,*,#3401,.F.);
#4389=ORIENTED_EDGE('',*,*,#3402,.F.);
#4390=ORIENTED_EDGE('',*,*,#3403,.T.);
#4391=ORIENTED_EDGE('',*,*,#3404,.T.);
#4392=ORIENTED_EDGE('',*,*,#3405,.T.);
#4393=ORIENTED_EDGE('',*,*,#3406,.T.);
#4394=ORIENTED_EDGE('',*,*,#3392,.T.);
#4395=ORIENTED_EDGE('',*,*,#3407,.T.);
#4396=ORIENTED_EDGE('',*,*,#3408,.T.);
#4397=ORIENTED_EDGE('',*,*,#3409,.T.);
#4398=ORIENTED_EDGE('',*,*,#3410,.T.);
#4399=ORIENTED_EDGE('',*,*,#3410,.F.);
#4400=ORIENTED_EDGE('',*,*,#3411,.T.);
#4401=ORIENTED_EDGE('',*,*,#3402,.T.);
#4402=ORIENTED_EDGE('',*,*,#3411,.F.);
#4403=ORIENTED_EDGE('',*,*,#3407,.F.);
#4404=ORIENTED_EDGE('',*,*,#3412,.T.);
#4405=ORIENTED_EDGE('',*,*,#3401,.T.);
#4406=ORIENTED_EDGE('',*,*,#3412,.F.);
#4407=ORIENTED_EDGE('',*,*,#3408,.F.);
#4408=ORIENTED_EDGE('',*,*,#3413,.T.);
#4409=ORIENTED_EDGE('',*,*,#3400,.T.);
#4410=ORIENTED_EDGE('',*,*,#3413,.F.);
#4411=ORIENTED_EDGE('',*,*,#3409,.F.);
#4412=ORIENTED_EDGE('',*,*,#3414,.T.);
#4413=ORIENTED_EDGE('',*,*,#3399,.T.);
#4414=ORIENTED_EDGE('',*,*,#3414,.F.);
#4415=ORIENTED_EDGE('',*,*,#3415,.F.);
#4416=ORIENTED_EDGE('',*,*,#3396,.T.);
#4417=ORIENTED_EDGE('',*,*,#3416,.F.);
#4418=ORIENTED_EDGE('',*,*,#3403,.F.);
#4419=ORIENTED_EDGE('',*,*,#3397,.T.);
#4420=ORIENTED_EDGE('',*,*,#3415,.T.);
#4421=ORIENTED_EDGE('',*,*,#3406,.F.);
#4422=ORIENTED_EDGE('',*,*,#3417,.T.);
#4423=ORIENTED_EDGE('',*,*,#3398,.T.);
#4424=ORIENTED_EDGE('',*,*,#3417,.F.);
#4425=ORIENTED_EDGE('',*,*,#3405,.F.);
#4426=ORIENTED_EDGE('',*,*,#3418,.T.);
#4427=ORIENTED_EDGE('',*,*,#3416,.T.);
#4428=ORIENTED_EDGE('',*,*,#3395,.T.);
#4429=ORIENTED_EDGE('',*,*,#3418,.F.);
#4430=ORIENTED_EDGE('',*,*,#3404,.F.);
#4431=ORIENTED_EDGE('',*,*,#3419,.T.);
#4432=ORIENTED_EDGE('',*,*,#3420,.T.);
#4433=ORIENTED_EDGE('',*,*,#3421,.T.);
#4434=ORIENTED_EDGE('',*,*,#3422,.T.);
#4435=ORIENTED_EDGE('',*,*,#3420,.F.);
#4436=ORIENTED_EDGE('',*,*,#3423,.T.);
#4437=ORIENTED_EDGE('',*,*,#3422,.F.);
#4438=ORIENTED_EDGE('',*,*,#3424,.T.);
#4439=ORIENTED_EDGE('',*,*,#3425,.T.);
#4440=ORIENTED_EDGE('',*,*,#3426,.T.);
#4441=ORIENTED_EDGE('',*,*,#3427,.T.);
#4442=ORIENTED_EDGE('',*,*,#3424,.F.);
#4443=ORIENTED_EDGE('',*,*,#3421,.F.);
#4444=ORIENTED_EDGE('',*,*,#3427,.F.);
#4445=ORIENTED_EDGE('',*,*,#3419,.F.);
#4446=ORIENTED_EDGE('',*,*,#3423,.F.);
#4447=ORIENTED_EDGE('',*,*,#3428,.T.);
#4448=ORIENTED_EDGE('',*,*,#3425,.F.);
#4449=ORIENTED_EDGE('',*,*,#3429,.T.);
#4450=ORIENTED_EDGE('',*,*,#3430,.T.);
#4451=ORIENTED_EDGE('',*,*,#3431,.T.);
#4452=ORIENTED_EDGE('',*,*,#3428,.F.);
#4453=ORIENTED_EDGE('',*,*,#3432,.T.);
#4454=ORIENTED_EDGE('',*,*,#3433,.F.);
#4455=ORIENTED_EDGE('',*,*,#3434,.F.);
#4456=ORIENTED_EDGE('',*,*,#3432,.F.);
#4457=ORIENTED_EDGE('',*,*,#3429,.F.);
#4458=ORIENTED_EDGE('',*,*,#3426,.F.);
#4459=ORIENTED_EDGE('',*,*,#3431,.F.);
#4460=ORIENTED_EDGE('',*,*,#3435,.T.);
#4461=ORIENTED_EDGE('',*,*,#3430,.F.);
#4462=ORIENTED_EDGE('',*,*,#3435,.F.);
#4463=ORIENTED_EDGE('',*,*,#3436,.T.);
#4464=ORIENTED_EDGE('',*,*,#3434,.T.);
#4465=ORIENTED_EDGE('',*,*,#3437,.T.);
#4466=ORIENTED_EDGE('',*,*,#3438,.T.);
#4467=ORIENTED_EDGE('',*,*,#3439,.T.);
#4468=ORIENTED_EDGE('',*,*,#3437,.F.);
#4469=ORIENTED_EDGE('',*,*,#3433,.T.);
#4470=ORIENTED_EDGE('',*,*,#3440,.F.);
#4471=ORIENTED_EDGE('',*,*,#3441,.F.);
#4472=ORIENTED_EDGE('',*,*,#3442,.T.);
#4473=ORIENTED_EDGE('',*,*,#3436,.F.);
#4474=ORIENTED_EDGE('',*,*,#3442,.F.);
#4475=ORIENTED_EDGE('',*,*,#3439,.F.);
#4476=ORIENTED_EDGE('',*,*,#3443,.T.);
#4477=ORIENTED_EDGE('',*,*,#3444,.T.);
#4478=ORIENTED_EDGE('',*,*,#3443,.F.);
#4479=ORIENTED_EDGE('',*,*,#3438,.F.);
#4480=ORIENTED_EDGE('',*,*,#3445,.T.);
#4481=ORIENTED_EDGE('',*,*,#3446,.T.);
#4482=ORIENTED_EDGE('',*,*,#3440,.T.);
#4483=ORIENTED_EDGE('',*,*,#3441,.T.);
#4484=ORIENTED_EDGE('',*,*,#3446,.F.);
#4485=ORIENTED_EDGE('',*,*,#3447,.T.);
#4486=ORIENTED_EDGE('',*,*,#3444,.F.);
#4487=ORIENTED_EDGE('',*,*,#3448,.T.);
#4488=ORIENTED_EDGE('',*,*,#3449,.T.);
#4489=ORIENTED_EDGE('',*,*,#3450,.T.);
#4490=ORIENTED_EDGE('',*,*,#3451,.T.);
#4491=ORIENTED_EDGE('',*,*,#3447,.F.);
#4492=ORIENTED_EDGE('',*,*,#3445,.F.);
#4493=ORIENTED_EDGE('',*,*,#3451,.F.);
#4494=ORIENTED_EDGE('',*,*,#3452,.T.);
#4495=ORIENTED_EDGE('',*,*,#3453,.T.);
#4496=ORIENTED_EDGE('',*,*,#3454,.T.);
#4497=ORIENTED_EDGE('',*,*,#3449,.F.);
#4498=ORIENTED_EDGE('',*,*,#3455,.T.);
#4499=ORIENTED_EDGE('',*,*,#3452,.F.);
#4500=ORIENTED_EDGE('',*,*,#3448,.F.);
#4501=ORIENTED_EDGE('',*,*,#3454,.F.);
#4502=ORIENTED_EDGE('',*,*,#3450,.F.);
#4503=ORIENTED_EDGE('',*,*,#3456,.T.);
#4504=ORIENTED_EDGE('',*,*,#3457,.T.);
#4505=ORIENTED_EDGE('',*,*,#3453,.F.);
#4506=ORIENTED_EDGE('',*,*,#3458,.T.);
#4507=ORIENTED_EDGE('',*,*,#3459,.F.);
#4508=ORIENTED_EDGE('',*,*,#3460,.F.);
#4509=ORIENTED_EDGE('',*,*,#3458,.F.);
#4510=ORIENTED_EDGE('',*,*,#3455,.F.);
#4511=ORIENTED_EDGE('',*,*,#3461,.T.);
#4512=ORIENTED_EDGE('',*,*,#3457,.F.);
#4513=ORIENTED_EDGE('',*,*,#3462,.T.);
#4514=ORIENTED_EDGE('',*,*,#3459,.T.);
#4515=ORIENTED_EDGE('',*,*,#3456,.F.);
#4516=ORIENTED_EDGE('',*,*,#3461,.F.);
#4517=ORIENTED_EDGE('',*,*,#3460,.T.);
#4518=ORIENTED_EDGE('',*,*,#3462,.F.);
#4519=ORIENTED_EDGE('',*,*,#3463,.T.);
#4520=ORIENTED_EDGE('',*,*,#3464,.T.);
#4521=ORIENTED_EDGE('',*,*,#3465,.T.);
#4522=ORIENTED_EDGE('',*,*,#3464,.F.);
#4523=ORIENTED_EDGE('',*,*,#3465,.F.);
#4524=ORIENTED_EDGE('',*,*,#3466,.T.);
#4525=ORIENTED_EDGE('',*,*,#3467,.F.);
#4526=ORIENTED_EDGE('',*,*,#3468,.F.);
#4527=ORIENTED_EDGE('',*,*,#3469,.F.);
#4528=ORIENTED_EDGE('',*,*,#3470,.F.);
#4529=ORIENTED_EDGE('',*,*,#3471,.F.);
#4530=ORIENTED_EDGE('',*,*,#3472,.F.);
#4531=ORIENTED_EDGE('',*,*,#3473,.F.);
#4532=ORIENTED_EDGE('',*,*,#3474,.F.);
#4533=ORIENTED_EDGE('',*,*,#3463,.F.);
#4534=ORIENTED_EDGE('',*,*,#3475,.F.);
#4535=ORIENTED_EDGE('',*,*,#3476,.T.);
#4536=ORIENTED_EDGE('',*,*,#3466,.F.);
#4537=ORIENTED_EDGE('',*,*,#3476,.F.);
#4538=ORIENTED_EDGE('',*,*,#3477,.F.);
#4539=ORIENTED_EDGE('',*,*,#3478,.T.);
#4540=ORIENTED_EDGE('',*,*,#3474,.T.);
#4541=ORIENTED_EDGE('',*,*,#3478,.F.);
#4542=ORIENTED_EDGE('',*,*,#3479,.F.);
#4543=ORIENTED_EDGE('',*,*,#3480,.T.);
#4544=ORIENTED_EDGE('',*,*,#3473,.T.);
#4545=ORIENTED_EDGE('',*,*,#3480,.F.);
#4546=ORIENTED_EDGE('',*,*,#3481,.F.);
#4547=ORIENTED_EDGE('',*,*,#3482,.T.);
#4548=ORIENTED_EDGE('',*,*,#3472,.T.);
#4549=ORIENTED_EDGE('',*,*,#3482,.F.);
#4550=ORIENTED_EDGE('',*,*,#3483,.F.);
#4551=ORIENTED_EDGE('',*,*,#3484,.T.);
#4552=ORIENTED_EDGE('',*,*,#3471,.T.);
#4553=ORIENTED_EDGE('',*,*,#3484,.F.);
#4554=ORIENTED_EDGE('',*,*,#3485,.F.);
#4555=ORIENTED_EDGE('',*,*,#3468,.T.);
#4556=ORIENTED_EDGE('',*,*,#3486,.F.);
#4557=ORIENTED_EDGE('',*,*,#3487,.F.);
#4558=ORIENTED_EDGE('',*,*,#3469,.T.);
#4559=ORIENTED_EDGE('',*,*,#3485,.T.);
#4560=ORIENTED_EDGE('',*,*,#3488,.T.);
#4561=ORIENTED_EDGE('',*,*,#3489,.T.);
#4562=ORIENTED_EDGE('',*,*,#3490,.T.);
#4563=ORIENTED_EDGE('',*,*,#3470,.T.);
#4564=ORIENTED_EDGE('',*,*,#3489,.F.);
#4565=ORIENTED_EDGE('',*,*,#3491,.T.);
#4566=ORIENTED_EDGE('',*,*,#3467,.T.);
#4567=ORIENTED_EDGE('',*,*,#3490,.F.);
#4568=ORIENTED_EDGE('',*,*,#3492,.F.);
#4569=ORIENTED_EDGE('',*,*,#3486,.T.);
#4570=ORIENTED_EDGE('',*,*,#3487,.T.);
#4571=ORIENTED_EDGE('',*,*,#3492,.T.);
#4572=ORIENTED_EDGE('',*,*,#3491,.F.);
#4573=ORIENTED_EDGE('',*,*,#3488,.F.);
#4574=ORIENTED_EDGE('',*,*,#3483,.T.);
#4575=ORIENTED_EDGE('',*,*,#3477,.T.);
#4576=ORIENTED_EDGE('',*,*,#3479,.T.);
#4577=ORIENTED_EDGE('',*,*,#3481,.T.);
#4578=ORIENTED_EDGE('',*,*,#3475,.T.);
#4579=ORIENTED_EDGE('',*,*,#3493,.T.);
#4580=ORIENTED_EDGE('',*,*,#3494,.T.);
#4581=ORIENTED_EDGE('',*,*,#3495,.T.);
#4582=ORIENTED_EDGE('',*,*,#3496,.T.);
#4583=ORIENTED_EDGE('',*,*,#3494,.F.);
#4584=ORIENTED_EDGE('',*,*,#3497,.T.);
#4585=ORIENTED_EDGE('',*,*,#3496,.F.);
#4586=ORIENTED_EDGE('',*,*,#3498,.T.);
#4587=ORIENTED_EDGE('',*,*,#3499,.T.);
#4588=ORIENTED_EDGE('',*,*,#3500,.T.);
#4589=ORIENTED_EDGE('',*,*,#3501,.T.);
#4590=ORIENTED_EDGE('',*,*,#3498,.F.);
#4591=ORIENTED_EDGE('',*,*,#3495,.F.);
#4592=ORIENTED_EDGE('',*,*,#3501,.F.);
#4593=ORIENTED_EDGE('',*,*,#3493,.F.);
#4594=ORIENTED_EDGE('',*,*,#3497,.F.);
#4595=ORIENTED_EDGE('',*,*,#3502,.T.);
#4596=ORIENTED_EDGE('',*,*,#3499,.F.);
#4597=ORIENTED_EDGE('',*,*,#3503,.T.);
#4598=ORIENTED_EDGE('',*,*,#3504,.T.);
#4599=ORIENTED_EDGE('',*,*,#3505,.T.);
#4600=ORIENTED_EDGE('',*,*,#3502,.F.);
#4601=ORIENTED_EDGE('',*,*,#3506,.T.);
#4602=ORIENTED_EDGE('',*,*,#3507,.F.);
#4603=ORIENTED_EDGE('',*,*,#3508,.F.);
#4604=ORIENTED_EDGE('',*,*,#3506,.F.);
#4605=ORIENTED_EDGE('',*,*,#3503,.F.);
#4606=ORIENTED_EDGE('',*,*,#3500,.F.);
#4607=ORIENTED_EDGE('',*,*,#3505,.F.);
#4608=ORIENTED_EDGE('',*,*,#3509,.T.);
#4609=ORIENTED_EDGE('',*,*,#3504,.F.);
#4610=ORIENTED_EDGE('',*,*,#3509,.F.);
#4611=ORIENTED_EDGE('',*,*,#3510,.T.);
#4612=ORIENTED_EDGE('',*,*,#3508,.T.);
#4613=ORIENTED_EDGE('',*,*,#3511,.T.);
#4614=ORIENTED_EDGE('',*,*,#3512,.T.);
#4615=ORIENTED_EDGE('',*,*,#3513,.T.);
#4616=ORIENTED_EDGE('',*,*,#3511,.F.);
#4617=ORIENTED_EDGE('',*,*,#3507,.T.);
#4618=ORIENTED_EDGE('',*,*,#3514,.F.);
#4619=ORIENTED_EDGE('',*,*,#3515,.F.);
#4620=ORIENTED_EDGE('',*,*,#3516,.T.);
#4621=ORIENTED_EDGE('',*,*,#3510,.F.);
#4622=ORIENTED_EDGE('',*,*,#3516,.F.);
#4623=ORIENTED_EDGE('',*,*,#3513,.F.);
#4624=ORIENTED_EDGE('',*,*,#3517,.T.);
#4625=ORIENTED_EDGE('',*,*,#3518,.T.);
#4626=ORIENTED_EDGE('',*,*,#3517,.F.);
#4627=ORIENTED_EDGE('',*,*,#3512,.F.);
#4628=ORIENTED_EDGE('',*,*,#3519,.T.);
#4629=ORIENTED_EDGE('',*,*,#3520,.T.);
#4630=ORIENTED_EDGE('',*,*,#3514,.T.);
#4631=ORIENTED_EDGE('',*,*,#3515,.T.);
#4632=ORIENTED_EDGE('',*,*,#3520,.F.);
#4633=ORIENTED_EDGE('',*,*,#3521,.T.);
#4634=ORIENTED_EDGE('',*,*,#3518,.F.);
#4635=ORIENTED_EDGE('',*,*,#3522,.T.);
#4636=ORIENTED_EDGE('',*,*,#3523,.T.);
#4637=ORIENTED_EDGE('',*,*,#3524,.T.);
#4638=ORIENTED_EDGE('',*,*,#3525,.T.);
#4639=ORIENTED_EDGE('',*,*,#3521,.F.);
#4640=ORIENTED_EDGE('',*,*,#3519,.F.);
#4641=ORIENTED_EDGE('',*,*,#3525,.F.);
#4642=ORIENTED_EDGE('',*,*,#3526,.T.);
#4643=ORIENTED_EDGE('',*,*,#3527,.T.);
#4644=ORIENTED_EDGE('',*,*,#3528,.T.);
#4645=ORIENTED_EDGE('',*,*,#3523,.F.);
#4646=ORIENTED_EDGE('',*,*,#3529,.T.);
#4647=ORIENTED_EDGE('',*,*,#3526,.F.);
#4648=ORIENTED_EDGE('',*,*,#3522,.F.);
#4649=ORIENTED_EDGE('',*,*,#3528,.F.);
#4650=ORIENTED_EDGE('',*,*,#3524,.F.);
#4651=ORIENTED_EDGE('',*,*,#3530,.T.);
#4652=ORIENTED_EDGE('',*,*,#3531,.T.);
#4653=ORIENTED_EDGE('',*,*,#3527,.F.);
#4654=ORIENTED_EDGE('',*,*,#3532,.T.);
#4655=ORIENTED_EDGE('',*,*,#3533,.F.);
#4656=ORIENTED_EDGE('',*,*,#3534,.F.);
#4657=ORIENTED_EDGE('',*,*,#3532,.F.);
#4658=ORIENTED_EDGE('',*,*,#3529,.F.);
#4659=ORIENTED_EDGE('',*,*,#3535,.T.);
#4660=ORIENTED_EDGE('',*,*,#3531,.F.);
#4661=ORIENTED_EDGE('',*,*,#3536,.T.);
#4662=ORIENTED_EDGE('',*,*,#3533,.T.);
#4663=ORIENTED_EDGE('',*,*,#3530,.F.);
#4664=ORIENTED_EDGE('',*,*,#3535,.F.);
#4665=ORIENTED_EDGE('',*,*,#3534,.T.);
#4666=ORIENTED_EDGE('',*,*,#3536,.F.);
#4667=ORIENTED_EDGE('',*,*,#3537,.F.);
#4668=ORIENTED_EDGE('',*,*,#3538,.T.);
#4669=ORIENTED_EDGE('',*,*,#3539,.F.);
#4670=ORIENTED_EDGE('',*,*,#3538,.F.);
#4671=ORIENTED_EDGE('',*,*,#3539,.T.);
#4672=ORIENTED_EDGE('',*,*,#3540,.F.);
#4673=ORIENTED_EDGE('',*,*,#3537,.T.);
#4674=ORIENTED_EDGE('',*,*,#3541,.T.);
#4675=ORIENTED_EDGE('',*,*,#3542,.T.);
#4676=ORIENTED_EDGE('',*,*,#3540,.T.);
#4677=ORIENTED_EDGE('',*,*,#3542,.F.);
#4678=ORIENTED_EDGE('',*,*,#3541,.F.);
#4679=ORIENTED_EDGE('',*,*,#3543,.T.);
#4680=ORIENTED_EDGE('',*,*,#3544,.T.);
#4681=ORIENTED_EDGE('',*,*,#3545,.T.);
#4682=ORIENTED_EDGE('',*,*,#3546,.T.);
#4683=ORIENTED_EDGE('',*,*,#3547,.T.);
#4684=ORIENTED_EDGE('',*,*,#3548,.T.);
#4685=ORIENTED_EDGE('',*,*,#3547,.F.);
#4686=ORIENTED_EDGE('',*,*,#3549,.T.);
#4687=ORIENTED_EDGE('',*,*,#3550,.T.);
#4688=ORIENTED_EDGE('',*,*,#3551,.T.);
#4689=ORIENTED_EDGE('',*,*,#3548,.F.);
#4690=ORIENTED_EDGE('',*,*,#3552,.T.);
#4691=ORIENTED_EDGE('',*,*,#3549,.F.);
#4692=ORIENTED_EDGE('',*,*,#3546,.F.);
#4693=ORIENTED_EDGE('',*,*,#3553,.T.);
#4694=ORIENTED_EDGE('',*,*,#3550,.F.);
#4695=ORIENTED_EDGE('',*,*,#3554,.T.);
#4696=ORIENTED_EDGE('',*,*,#3555,.T.);
#4697=ORIENTED_EDGE('',*,*,#3551,.F.);
#4698=ORIENTED_EDGE('',*,*,#3556,.T.);
#4699=ORIENTED_EDGE('',*,*,#3557,.T.);
#4700=ORIENTED_EDGE('',*,*,#3543,.F.);
#4701=ORIENTED_EDGE('',*,*,#3558,.T.);
#4702=ORIENTED_EDGE('',*,*,#3544,.F.);
#4703=ORIENTED_EDGE('',*,*,#3559,.T.);
#4704=ORIENTED_EDGE('',*,*,#3560,.T.);
#4705=ORIENTED_EDGE('',*,*,#3545,.F.);
#4706=ORIENTED_EDGE('',*,*,#3561,.T.);
#4707=ORIENTED_EDGE('',*,*,#3562,.F.);
#4708=ORIENTED_EDGE('',*,*,#3563,.F.);
#4709=ORIENTED_EDGE('',*,*,#3564,.F.);
#4710=ORIENTED_EDGE('',*,*,#3554,.F.);
#4711=ORIENTED_EDGE('',*,*,#3552,.F.);
#4712=ORIENTED_EDGE('',*,*,#3560,.F.);
#4713=ORIENTED_EDGE('',*,*,#3553,.F.);
#4714=ORIENTED_EDGE('',*,*,#3564,.T.);
#4715=ORIENTED_EDGE('',*,*,#3565,.F.);
#4716=ORIENTED_EDGE('',*,*,#3566,.F.);
#4717=ORIENTED_EDGE('',*,*,#3556,.F.);
#4718=ORIENTED_EDGE('',*,*,#3567,.T.);
#4719=ORIENTED_EDGE('',*,*,#3568,.T.);
#4720=ORIENTED_EDGE('',*,*,#3559,.F.);
#4721=ORIENTED_EDGE('',*,*,#3557,.F.);
#4722=ORIENTED_EDGE('',*,*,#3555,.F.);
#4723=ORIENTED_EDGE('',*,*,#3566,.T.);
#4724=ORIENTED_EDGE('',*,*,#3562,.T.);
#4725=ORIENTED_EDGE('',*,*,#3561,.F.);
#4726=ORIENTED_EDGE('',*,*,#3558,.F.);
#4727=ORIENTED_EDGE('',*,*,#3568,.F.);
#4728=ORIENTED_EDGE('',*,*,#3569,.T.);
#4729=ORIENTED_EDGE('',*,*,#3565,.T.);
#4730=ORIENTED_EDGE('',*,*,#3563,.T.);
#4731=ORIENTED_EDGE('',*,*,#3569,.F.);
#4732=ORIENTED_EDGE('',*,*,#3567,.F.);
#4733=ORIENTED_EDGE('',*,*,#3570,.F.);
#4734=ORIENTED_EDGE('',*,*,#3571,.T.);
#4735=ORIENTED_EDGE('',*,*,#3572,.F.);
#4736=ORIENTED_EDGE('',*,*,#3571,.F.);
#4737=ORIENTED_EDGE('',*,*,#3572,.T.);
#4738=ORIENTED_EDGE('',*,*,#3573,.F.);
#4739=ORIENTED_EDGE('',*,*,#3570,.T.);
#4740=ORIENTED_EDGE('',*,*,#3574,.T.);
#4741=ORIENTED_EDGE('',*,*,#3575,.T.);
#4742=ORIENTED_EDGE('',*,*,#3573,.T.);
#4743=ORIENTED_EDGE('',*,*,#3575,.F.);
#4744=ORIENTED_EDGE('',*,*,#3574,.F.);
#4745=ORIENTED_EDGE('',*,*,#3576,.T.);
#4746=ORIENTED_EDGE('',*,*,#3577,.T.);
#4747=ORIENTED_EDGE('',*,*,#3578,.T.);
#4748=ORIENTED_EDGE('',*,*,#3579,.T.);
#4749=ORIENTED_EDGE('',*,*,#3580,.T.);
#4750=ORIENTED_EDGE('',*,*,#3581,.T.);
#4751=ORIENTED_EDGE('',*,*,#3580,.F.);
#4752=ORIENTED_EDGE('',*,*,#3582,.T.);
#4753=ORIENTED_EDGE('',*,*,#3583,.T.);
#4754=ORIENTED_EDGE('',*,*,#3584,.T.);
#4755=ORIENTED_EDGE('',*,*,#3581,.F.);
#4756=ORIENTED_EDGE('',*,*,#3585,.T.);
#4757=ORIENTED_EDGE('',*,*,#3582,.F.);
#4758=ORIENTED_EDGE('',*,*,#3579,.F.);
#4759=ORIENTED_EDGE('',*,*,#3586,.T.);
#4760=ORIENTED_EDGE('',*,*,#3583,.F.);
#4761=ORIENTED_EDGE('',*,*,#3587,.T.);
#4762=ORIENTED_EDGE('',*,*,#3588,.T.);
#4763=ORIENTED_EDGE('',*,*,#3584,.F.);
#4764=ORIENTED_EDGE('',*,*,#3589,.T.);
#4765=ORIENTED_EDGE('',*,*,#3590,.T.);
#4766=ORIENTED_EDGE('',*,*,#3576,.F.);
#4767=ORIENTED_EDGE('',*,*,#3591,.T.);
#4768=ORIENTED_EDGE('',*,*,#3577,.F.);
#4769=ORIENTED_EDGE('',*,*,#3592,.T.);
#4770=ORIENTED_EDGE('',*,*,#3593,.T.);
#4771=ORIENTED_EDGE('',*,*,#3578,.F.);
#4772=ORIENTED_EDGE('',*,*,#3594,.T.);
#4773=ORIENTED_EDGE('',*,*,#3595,.F.);
#4774=ORIENTED_EDGE('',*,*,#3596,.F.);
#4775=ORIENTED_EDGE('',*,*,#3597,.F.);
#4776=ORIENTED_EDGE('',*,*,#3587,.F.);
#4777=ORIENTED_EDGE('',*,*,#3585,.F.);
#4778=ORIENTED_EDGE('',*,*,#3593,.F.);
#4779=ORIENTED_EDGE('',*,*,#3586,.F.);
#4780=ORIENTED_EDGE('',*,*,#3597,.T.);
#4781=ORIENTED_EDGE('',*,*,#3598,.F.);
#4782=ORIENTED_EDGE('',*,*,#3599,.F.);
#4783=ORIENTED_EDGE('',*,*,#3589,.F.);
#4784=ORIENTED_EDGE('',*,*,#3600,.T.);
#4785=ORIENTED_EDGE('',*,*,#3601,.T.);
#4786=ORIENTED_EDGE('',*,*,#3592,.F.);
#4787=ORIENTED_EDGE('',*,*,#3590,.F.);
#4788=ORIENTED_EDGE('',*,*,#3588,.F.);
#4789=ORIENTED_EDGE('',*,*,#3599,.T.);
#4790=ORIENTED_EDGE('',*,*,#3595,.T.);
#4791=ORIENTED_EDGE('',*,*,#3594,.F.);
#4792=ORIENTED_EDGE('',*,*,#3591,.F.);
#4793=ORIENTED_EDGE('',*,*,#3601,.F.);
#4794=ORIENTED_EDGE('',*,*,#3602,.T.);
#4795=ORIENTED_EDGE('',*,*,#3598,.T.);
#4796=ORIENTED_EDGE('',*,*,#3596,.T.);
#4797=ORIENTED_EDGE('',*,*,#3602,.F.);
#4798=ORIENTED_EDGE('',*,*,#3600,.F.);
#4799=ORIENTED_EDGE('',*,*,#3603,.T.);
#4800=ORIENTED_EDGE('',*,*,#3604,.T.);
#4801=ORIENTED_EDGE('',*,*,#3605,.T.);
#4802=ORIENTED_EDGE('',*,*,#3606,.T.);
#4803=ORIENTED_EDGE('',*,*,#3607,.T.);
#4804=ORIENTED_EDGE('',*,*,#3608,.T.);
#4805=ORIENTED_EDGE('',*,*,#3607,.F.);
#4806=ORIENTED_EDGE('',*,*,#3609,.T.);
#4807=ORIENTED_EDGE('',*,*,#3610,.T.);
#4808=ORIENTED_EDGE('',*,*,#3611,.T.);
#4809=ORIENTED_EDGE('',*,*,#3608,.F.);
#4810=ORIENTED_EDGE('',*,*,#3612,.T.);
#4811=ORIENTED_EDGE('',*,*,#3609,.F.);
#4812=ORIENTED_EDGE('',*,*,#3606,.F.);
#4813=ORIENTED_EDGE('',*,*,#3613,.T.);
#4814=ORIENTED_EDGE('',*,*,#3610,.F.);
#4815=ORIENTED_EDGE('',*,*,#3614,.T.);
#4816=ORIENTED_EDGE('',*,*,#3615,.T.);
#4817=ORIENTED_EDGE('',*,*,#3611,.F.);
#4818=ORIENTED_EDGE('',*,*,#3616,.T.);
#4819=ORIENTED_EDGE('',*,*,#3617,.T.);
#4820=ORIENTED_EDGE('',*,*,#3603,.F.);
#4821=ORIENTED_EDGE('',*,*,#3618,.T.);
#4822=ORIENTED_EDGE('',*,*,#3604,.F.);
#4823=ORIENTED_EDGE('',*,*,#3619,.T.);
#4824=ORIENTED_EDGE('',*,*,#3620,.T.);
#4825=ORIENTED_EDGE('',*,*,#3605,.F.);
#4826=ORIENTED_EDGE('',*,*,#3621,.T.);
#4827=ORIENTED_EDGE('',*,*,#3622,.F.);
#4828=ORIENTED_EDGE('',*,*,#3623,.F.);
#4829=ORIENTED_EDGE('',*,*,#3624,.F.);
#4830=ORIENTED_EDGE('',*,*,#3614,.F.);
#4831=ORIENTED_EDGE('',*,*,#3612,.F.);
#4832=ORIENTED_EDGE('',*,*,#3620,.F.);
#4833=ORIENTED_EDGE('',*,*,#3613,.F.);
#4834=ORIENTED_EDGE('',*,*,#3624,.T.);
#4835=ORIENTED_EDGE('',*,*,#3625,.F.);
#4836=ORIENTED_EDGE('',*,*,#3626,.F.);
#4837=ORIENTED_EDGE('',*,*,#3616,.F.);
#4838=ORIENTED_EDGE('',*,*,#3627,.T.);
#4839=ORIENTED_EDGE('',*,*,#3628,.T.);
#4840=ORIENTED_EDGE('',*,*,#3619,.F.);
#4841=ORIENTED_EDGE('',*,*,#3617,.F.);
#4842=ORIENTED_EDGE('',*,*,#3615,.F.);
#4843=ORIENTED_EDGE('',*,*,#3626,.T.);
#4844=ORIENTED_EDGE('',*,*,#3622,.T.);
#4845=ORIENTED_EDGE('',*,*,#3621,.F.);
#4846=ORIENTED_EDGE('',*,*,#3618,.F.);
#4847=ORIENTED_EDGE('',*,*,#3628,.F.);
#4848=ORIENTED_EDGE('',*,*,#3629,.T.);
#4849=ORIENTED_EDGE('',*,*,#3625,.T.);
#4850=ORIENTED_EDGE('',*,*,#3623,.T.);
#4851=ORIENTED_EDGE('',*,*,#3629,.F.);
#4852=ORIENTED_EDGE('',*,*,#3627,.F.);
#4853=ORIENTED_EDGE('',*,*,#3630,.F.);
#4854=ORIENTED_EDGE('',*,*,#3631,.T.);
#4855=ORIENTED_EDGE('',*,*,#3632,.F.);
#4856=ORIENTED_EDGE('',*,*,#3631,.F.);
#4857=ORIENTED_EDGE('',*,*,#3632,.T.);
#4858=ORIENTED_EDGE('',*,*,#3633,.F.);
#4859=ORIENTED_EDGE('',*,*,#3630,.T.);
#4860=ORIENTED_EDGE('',*,*,#3634,.T.);
#4861=ORIENTED_EDGE('',*,*,#3635,.T.);
#4862=ORIENTED_EDGE('',*,*,#3633,.T.);
#4863=ORIENTED_EDGE('',*,*,#3635,.F.);
#4864=ORIENTED_EDGE('',*,*,#3634,.F.);
#4865=ORIENTED_EDGE('',*,*,#3636,.F.);
#4866=ORIENTED_EDGE('',*,*,#3637,.T.);
#4867=ORIENTED_EDGE('',*,*,#3638,.F.);
#4868=ORIENTED_EDGE('',*,*,#3639,.F.);
#4869=ORIENTED_EDGE('',*,*,#3637,.F.);
#4870=ORIENTED_EDGE('',*,*,#3640,.F.);
#4871=ORIENTED_EDGE('',*,*,#3641,.F.);
#4872=ORIENTED_EDGE('',*,*,#3642,.T.);
#4873=ORIENTED_EDGE('',*,*,#3643,.F.);
#4874=ORIENTED_EDGE('',*,*,#3644,.F.);
#4875=ORIENTED_EDGE('',*,*,#3642,.F.);
#4876=ORIENTED_EDGE('',*,*,#3645,.F.);
#4877=ORIENTED_EDGE('',*,*,#3646,.T.);
#4878=ORIENTED_EDGE('',*,*,#3647,.F.);
#4879=ORIENTED_EDGE('',*,*,#3646,.F.);
#4880=ORIENTED_EDGE('',*,*,#3648,.F.);
#4881=ORIENTED_EDGE('',*,*,#3649,.F.);
#4882=ORIENTED_EDGE('',*,*,#3650,.T.);
#4883=ORIENTED_EDGE('',*,*,#3651,.F.);
#4884=ORIENTED_EDGE('',*,*,#3650,.F.);
#4885=ORIENTED_EDGE('',*,*,#3652,.F.);
#4886=ORIENTED_EDGE('',*,*,#3653,.T.);
#4887=ORIENTED_EDGE('',*,*,#3654,.F.);
#4888=ORIENTED_EDGE('',*,*,#3653,.F.);
#4889=ORIENTED_EDGE('',*,*,#3655,.F.);
#4890=ORIENTED_EDGE('',*,*,#3641,.T.);
#4891=ORIENTED_EDGE('',*,*,#3643,.T.);
#4892=ORIENTED_EDGE('',*,*,#3644,.T.);
#4893=ORIENTED_EDGE('',*,*,#3656,.T.);
#4894=ORIENTED_EDGE('',*,*,#3640,.T.);
#4895=ORIENTED_EDGE('',*,*,#3636,.T.);
#4896=ORIENTED_EDGE('',*,*,#3656,.F.);
#4897=ORIENTED_EDGE('',*,*,#3657,.T.);
#4898=ORIENTED_EDGE('',*,*,#3658,.T.);
#4899=ORIENTED_EDGE('',*,*,#3655,.T.);
#4900=ORIENTED_EDGE('',*,*,#3658,.F.);
#4901=ORIENTED_EDGE('',*,*,#3638,.T.);
#4902=ORIENTED_EDGE('',*,*,#3639,.T.);
#4903=ORIENTED_EDGE('',*,*,#3659,.T.);
#4904=ORIENTED_EDGE('',*,*,#3648,.T.);
#4905=ORIENTED_EDGE('',*,*,#3645,.T.);
#4906=ORIENTED_EDGE('',*,*,#3659,.F.);
#4907=ORIENTED_EDGE('',*,*,#3657,.F.);
#4908=ORIENTED_EDGE('',*,*,#3652,.T.);
#4909=ORIENTED_EDGE('',*,*,#3649,.T.);
#4910=ORIENTED_EDGE('',*,*,#3660,.T.);
#4911=ORIENTED_EDGE('',*,*,#3654,.T.);
#4912=ORIENTED_EDGE('',*,*,#3660,.F.);
#4913=ORIENTED_EDGE('',*,*,#3647,.T.);
#4914=ORIENTED_EDGE('',*,*,#3651,.T.);
#4915=ORIENTED_EDGE('',*,*,#3661,.F.);
#4916=ORIENTED_EDGE('',*,*,#3662,.T.);
#4917=ORIENTED_EDGE('',*,*,#3663,.F.);
#4918=ORIENTED_EDGE('',*,*,#3662,.F.);
#4919=ORIENTED_EDGE('',*,*,#3664,.F.);
#4920=ORIENTED_EDGE('',*,*,#3665,.F.);
#4921=ORIENTED_EDGE('',*,*,#3666,.F.);
#4922=ORIENTED_EDGE('',*,*,#3667,.F.);
#4923=ORIENTED_EDGE('',*,*,#3663,.T.);
#4924=ORIENTED_EDGE('',*,*,#3668,.F.);
#4925=ORIENTED_EDGE('',*,*,#3669,.F.);
#4926=ORIENTED_EDGE('',*,*,#3670,.F.);
#4927=ORIENTED_EDGE('',*,*,#3671,.F.);
#4928=ORIENTED_EDGE('',*,*,#3672,.F.);
#4929=ORIENTED_EDGE('',*,*,#3673,.F.);
#4930=ORIENTED_EDGE('',*,*,#3674,.F.);
#4931=ORIENTED_EDGE('',*,*,#3675,.F.);
#4932=ORIENTED_EDGE('',*,*,#3676,.T.);
#4933=ORIENTED_EDGE('',*,*,#3677,.T.);
#4934=ORIENTED_EDGE('',*,*,#3678,.T.);
#4935=ORIENTED_EDGE('',*,*,#3679,.T.);
#4936=ORIENTED_EDGE('',*,*,#3680,.T.);
#4937=ORIENTED_EDGE('',*,*,#3681,.T.);
#4938=ORIENTED_EDGE('',*,*,#3682,.T.);
#4939=ORIENTED_EDGE('',*,*,#3683,.T.);
#4940=ORIENTED_EDGE('',*,*,#3661,.T.);
#4941=ORIENTED_EDGE('',*,*,#3684,.T.);
#4942=ORIENTED_EDGE('',*,*,#3685,.T.);
#4943=ORIENTED_EDGE('',*,*,#3686,.T.);
#4944=ORIENTED_EDGE('',*,*,#3687,.T.);
#4945=ORIENTED_EDGE('',*,*,#3688,.T.);
#4946=ORIENTED_EDGE('',*,*,#3689,.T.);
#4947=ORIENTED_EDGE('',*,*,#3690,.T.);
#4948=ORIENTED_EDGE('',*,*,#3691,.T.);
#4949=ORIENTED_EDGE('',*,*,#3691,.F.);
#4950=ORIENTED_EDGE('',*,*,#3692,.T.);
#4951=ORIENTED_EDGE('',*,*,#3675,.T.);
#4952=ORIENTED_EDGE('',*,*,#3692,.F.);
#4953=ORIENTED_EDGE('',*,*,#3684,.F.);
#4954=ORIENTED_EDGE('',*,*,#3693,.T.);
#4955=ORIENTED_EDGE('',*,*,#3674,.T.);
#4956=ORIENTED_EDGE('',*,*,#3693,.F.);
#4957=ORIENTED_EDGE('',*,*,#3673,.T.);
#4958=ORIENTED_EDGE('',*,*,#3694,.T.);
#4959=ORIENTED_EDGE('',*,*,#3689,.F.);
#4960=ORIENTED_EDGE('',*,*,#3694,.F.);
#4961=ORIENTED_EDGE('',*,*,#3672,.T.);
#4962=ORIENTED_EDGE('',*,*,#3695,.T.);
#4963=ORIENTED_EDGE('',*,*,#3688,.F.);
#4964=ORIENTED_EDGE('',*,*,#3695,.F.);
#4965=ORIENTED_EDGE('',*,*,#3671,.T.);
#4966=ORIENTED_EDGE('',*,*,#3696,.T.);
#4967=ORIENTED_EDGE('',*,*,#3687,.F.);
#4968=ORIENTED_EDGE('',*,*,#3696,.F.);
#4969=ORIENTED_EDGE('',*,*,#3670,.T.);
#4970=ORIENTED_EDGE('',*,*,#3697,.T.);
#4971=ORIENTED_EDGE('',*,*,#3686,.F.);
#4972=ORIENTED_EDGE('',*,*,#3697,.F.);
#4973=ORIENTED_EDGE('',*,*,#3685,.F.);
#4974=ORIENTED_EDGE('',*,*,#3698,.T.);
#4975=ORIENTED_EDGE('',*,*,#3669,.T.);
#4976=ORIENTED_EDGE('',*,*,#3698,.F.);
#4977=ORIENTED_EDGE('',*,*,#3690,.F.);
#4978=ORIENTED_EDGE('',*,*,#3699,.T.);
#4979=ORIENTED_EDGE('',*,*,#3668,.T.);
#4980=ORIENTED_EDGE('',*,*,#3699,.F.);
#4981=ORIENTED_EDGE('',*,*,#3700,.F.);
#4982=ORIENTED_EDGE('',*,*,#3701,.F.);
#4983=ORIENTED_EDGE('',*,*,#3702,.F.);
#4984=ORIENTED_EDGE('',*,*,#3703,.F.);
#4985=ORIENTED_EDGE('',*,*,#3678,.F.);
#4986=ORIENTED_EDGE('',*,*,#3704,.F.);
#4987=ORIENTED_EDGE('',*,*,#3665,.T.);
#4988=ORIENTED_EDGE('',*,*,#3705,.F.);
#4989=ORIENTED_EDGE('',*,*,#3666,.T.);
#4990=ORIENTED_EDGE('',*,*,#3704,.T.);
#4991=ORIENTED_EDGE('',*,*,#3677,.F.);
#4992=ORIENTED_EDGE('',*,*,#3706,.F.);
#4993=ORIENTED_EDGE('',*,*,#3706,.T.);
#4994=ORIENTED_EDGE('',*,*,#3676,.F.);
#4995=ORIENTED_EDGE('',*,*,#3707,.F.);
#4996=ORIENTED_EDGE('',*,*,#3667,.T.);
#4997=ORIENTED_EDGE('',*,*,#3664,.T.);
#4998=ORIENTED_EDGE('',*,*,#3707,.T.);
#4999=ORIENTED_EDGE('',*,*,#3683,.F.);
#5000=ORIENTED_EDGE('',*,*,#3708,.F.);
#5001=ORIENTED_EDGE('',*,*,#3709,.F.);
#5002=ORIENTED_EDGE('',*,*,#3710,.F.);
#5003=ORIENTED_EDGE('',*,*,#3711,.F.);
#5004=ORIENTED_EDGE('',*,*,#3705,.T.);
#5005=ORIENTED_EDGE('',*,*,#3708,.T.);
#5006=ORIENTED_EDGE('',*,*,#3682,.F.);
#5007=ORIENTED_EDGE('',*,*,#3712,.F.);
#5008=ORIENTED_EDGE('',*,*,#3713,.F.);
#5009=ORIENTED_EDGE('',*,*,#3712,.T.);
#5010=ORIENTED_EDGE('',*,*,#3681,.F.);
#5011=ORIENTED_EDGE('',*,*,#3714,.T.);
#5012=ORIENTED_EDGE('',*,*,#3715,.T.);
#5013=ORIENTED_EDGE('',*,*,#3680,.F.);
#5014=ORIENTED_EDGE('',*,*,#3716,.T.);
#5015=ORIENTED_EDGE('',*,*,#3717,.T.);
#5016=ORIENTED_EDGE('',*,*,#3714,.F.);
#5017=ORIENTED_EDGE('',*,*,#3703,.T.);
#5018=ORIENTED_EDGE('',*,*,#3718,.T.);
#5019=ORIENTED_EDGE('',*,*,#3716,.F.);
#5020=ORIENTED_EDGE('',*,*,#3679,.F.);
#5021=ORIENTED_EDGE('',*,*,#3719,.F.);
#5022=ORIENTED_EDGE('',*,*,#3720,.F.);
#5023=ORIENTED_EDGE('',*,*,#3701,.T.);
#5024=ORIENTED_EDGE('',*,*,#3721,.F.);
#5025=ORIENTED_EDGE('',*,*,#3702,.T.);
#5026=ORIENTED_EDGE('',*,*,#3720,.T.);
#5027=ORIENTED_EDGE('',*,*,#3722,.F.);
#5028=ORIENTED_EDGE('',*,*,#3709,.T.);
#5029=ORIENTED_EDGE('',*,*,#3713,.T.);
#5030=ORIENTED_EDGE('',*,*,#3715,.F.);
#5031=ORIENTED_EDGE('',*,*,#3717,.F.);
#5032=ORIENTED_EDGE('',*,*,#3718,.F.);
#5033=ORIENTED_EDGE('',*,*,#3723,.F.);
#5034=ORIENTED_EDGE('',*,*,#3724,.F.);
#5035=ORIENTED_EDGE('',*,*,#3725,.F.);
#5036=ORIENTED_EDGE('',*,*,#3726,.F.);
#5037=ORIENTED_EDGE('',*,*,#3727,.F.);
#5038=ORIENTED_EDGE('',*,*,#3728,.F.);
#5039=ORIENTED_EDGE('',*,*,#3729,.F.);
#5040=ORIENTED_EDGE('',*,*,#3730,.F.);
#5041=ORIENTED_EDGE('',*,*,#3731,.F.);
#5042=ORIENTED_EDGE('',*,*,#3700,.T.);
#5043=ORIENTED_EDGE('',*,*,#3711,.T.);
#5044=ORIENTED_EDGE('',*,*,#3732,.T.);
#5045=ORIENTED_EDGE('',*,*,#3721,.T.);
#5046=ORIENTED_EDGE('',*,*,#3733,.T.);
#5047=ORIENTED_EDGE('',*,*,#3734,.T.);
#5048=ORIENTED_EDGE('',*,*,#3735,.T.);
#5049=ORIENTED_EDGE('',*,*,#3736,.T.);
#5050=ORIENTED_EDGE('',*,*,#3737,.T.);
#5051=ORIENTED_EDGE('',*,*,#3738,.T.);
#5052=ORIENTED_EDGE('',*,*,#3739,.T.);
#5053=ORIENTED_EDGE('',*,*,#3740,.T.);
#5054=ORIENTED_EDGE('',*,*,#3741,.T.);
#5055=ORIENTED_EDGE('',*,*,#3732,.F.);
#5056=ORIENTED_EDGE('',*,*,#3710,.T.);
#5057=ORIENTED_EDGE('',*,*,#3722,.T.);
#5058=ORIENTED_EDGE('',*,*,#3719,.T.);
#5059=ORIENTED_EDGE('',*,*,#3741,.F.);
#5060=ORIENTED_EDGE('',*,*,#3742,.T.);
#5061=ORIENTED_EDGE('',*,*,#3731,.T.);
#5062=ORIENTED_EDGE('',*,*,#3742,.F.);
#5063=ORIENTED_EDGE('',*,*,#3734,.F.);
#5064=ORIENTED_EDGE('',*,*,#3743,.T.);
#5065=ORIENTED_EDGE('',*,*,#3730,.T.);
#5066=ORIENTED_EDGE('',*,*,#3743,.F.);
#5067=ORIENTED_EDGE('',*,*,#3729,.T.);
#5068=ORIENTED_EDGE('',*,*,#3744,.T.);
#5069=ORIENTED_EDGE('',*,*,#3739,.F.);
#5070=ORIENTED_EDGE('',*,*,#3744,.F.);
#5071=ORIENTED_EDGE('',*,*,#3728,.T.);
#5072=ORIENTED_EDGE('',*,*,#3745,.T.);
#5073=ORIENTED_EDGE('',*,*,#3738,.F.);
#5074=ORIENTED_EDGE('',*,*,#3745,.F.);
#5075=ORIENTED_EDGE('',*,*,#3727,.T.);
#5076=ORIENTED_EDGE('',*,*,#3746,.T.);
#5077=ORIENTED_EDGE('',*,*,#3737,.F.);
#5078=ORIENTED_EDGE('',*,*,#3746,.F.);
#5079=ORIENTED_EDGE('',*,*,#3726,.T.);
#5080=ORIENTED_EDGE('',*,*,#3747,.T.);
#5081=ORIENTED_EDGE('',*,*,#3736,.F.);
#5082=ORIENTED_EDGE('',*,*,#3747,.F.);
#5083=ORIENTED_EDGE('',*,*,#3735,.F.);
#5084=ORIENTED_EDGE('',*,*,#3748,.T.);
#5085=ORIENTED_EDGE('',*,*,#3725,.T.);
#5086=ORIENTED_EDGE('',*,*,#3748,.F.);
#5087=ORIENTED_EDGE('',*,*,#3740,.F.);
#5088=ORIENTED_EDGE('',*,*,#3749,.T.);
#5089=ORIENTED_EDGE('',*,*,#3724,.T.);
#5090=ORIENTED_EDGE('',*,*,#3749,.F.);
#5091=ORIENTED_EDGE('',*,*,#3733,.F.);
#5092=ORIENTED_EDGE('',*,*,#3750,.T.);
#5093=ORIENTED_EDGE('',*,*,#3723,.T.);
#5094=ORIENTED_EDGE('',*,*,#3750,.F.);
#5095=ORIENTED_EDGE('',*,*,#3751,.T.);
#5096=ORIENTED_EDGE('',*,*,#3752,.T.);
#5097=ORIENTED_EDGE('',*,*,#3753,.T.);
#5098=ORIENTED_EDGE('',*,*,#3752,.F.);
#5099=ORIENTED_EDGE('',*,*,#3753,.F.);
#5100=ORIENTED_EDGE('',*,*,#3754,.T.);
#5101=ORIENTED_EDGE('',*,*,#3751,.F.);
#5102=ORIENTED_EDGE('',*,*,#3755,.T.);
#5103=ORIENTED_EDGE('',*,*,#3756,.T.);
#5104=ORIENTED_EDGE('',*,*,#3754,.F.);
#5105=ORIENTED_EDGE('',*,*,#3756,.F.);
#5106=ORIENTED_EDGE('',*,*,#3755,.F.);
#5107=ORIENTED_EDGE('',*,*,#3757,.F.);
#5108=ORIENTED_EDGE('',*,*,#3758,.T.);
#5109=ORIENTED_EDGE('',*,*,#3759,.T.);
#5110=ORIENTED_EDGE('',*,*,#3757,.T.);
#5111=ORIENTED_EDGE('',*,*,#3759,.F.);
#5112=ORIENTED_EDGE('',*,*,#3758,.F.);
#5113=ORIENTED_EDGE('',*,*,#3760,.F.);
#5114=ORIENTED_EDGE('',*,*,#3761,.T.);
#5115=ORIENTED_EDGE('',*,*,#3762,.F.);
#5116=ORIENTED_EDGE('',*,*,#3761,.F.);
#5117=ORIENTED_EDGE('',*,*,#3763,.T.);
#5118=ORIENTED_EDGE('',*,*,#3764,.T.);
#5119=ORIENTED_EDGE('',*,*,#3765,.T.);
#5120=ORIENTED_EDGE('',*,*,#3766,.T.);
#5121=ORIENTED_EDGE('',*,*,#3767,.T.);
#5122=ORIENTED_EDGE('',*,*,#3760,.T.);
#5123=ORIENTED_EDGE('',*,*,#3767,.F.);
#5124=ORIENTED_EDGE('',*,*,#3768,.T.);
#5125=ORIENTED_EDGE('',*,*,#3769,.F.);
#5126=ORIENTED_EDGE('',*,*,#3768,.F.);
#5127=ORIENTED_EDGE('',*,*,#3770,.F.);
#5128=ORIENTED_EDGE('',*,*,#3771,.F.);
#5129=ORIENTED_EDGE('',*,*,#3772,.F.);
#5130=ORIENTED_EDGE('',*,*,#3766,.F.);
#5131=ORIENTED_EDGE('',*,*,#3773,.T.);
#5132=ORIENTED_EDGE('',*,*,#3774,.T.);
#5133=ORIENTED_EDGE('',*,*,#3770,.T.);
#5134=ORIENTED_EDGE('',*,*,#3765,.F.);
#5135=ORIENTED_EDGE('',*,*,#3775,.F.);
#5136=ORIENTED_EDGE('',*,*,#3776,.F.);
#5137=ORIENTED_EDGE('',*,*,#3773,.F.);
#5138=ORIENTED_EDGE('',*,*,#3764,.F.);
#5139=ORIENTED_EDGE('',*,*,#3772,.T.);
#5140=ORIENTED_EDGE('',*,*,#3777,.F.);
#5141=ORIENTED_EDGE('',*,*,#3775,.T.);
#5142=ORIENTED_EDGE('',*,*,#3763,.F.);
#5143=ORIENTED_EDGE('',*,*,#3776,.T.);
#5144=ORIENTED_EDGE('',*,*,#3777,.T.);
#5145=ORIENTED_EDGE('',*,*,#3771,.T.);
#5146=ORIENTED_EDGE('',*,*,#3774,.F.);
#5147=ORIENTED_EDGE('',*,*,#3769,.T.);
#5148=ORIENTED_EDGE('',*,*,#3762,.T.);
#5149=ORIENTED_EDGE('',*,*,#3778,.F.);
#5150=ORIENTED_EDGE('',*,*,#3779,.F.);
#5151=ORIENTED_EDGE('',*,*,#3780,.F.);
#5152=ORIENTED_EDGE('',*,*,#3781,.F.);
#5153=ORIENTED_EDGE('',*,*,#3782,.F.);
#5154=ORIENTED_EDGE('',*,*,#3783,.F.);
#5155=ORIENTED_EDGE('',*,*,#3784,.F.);
#5156=ORIENTED_EDGE('',*,*,#3779,.T.);
#5157=ORIENTED_EDGE('',*,*,#3784,.T.);
#5158=ORIENTED_EDGE('',*,*,#3785,.F.);
#5159=ORIENTED_EDGE('',*,*,#3786,.F.);
#5160=ORIENTED_EDGE('',*,*,#3780,.T.);
#5161=ORIENTED_EDGE('',*,*,#3782,.T.);
#5162=ORIENTED_EDGE('',*,*,#3778,.T.);
#5163=ORIENTED_EDGE('',*,*,#3787,.T.);
#5164=ORIENTED_EDGE('',*,*,#3788,.T.);
#5165=ORIENTED_EDGE('',*,*,#3788,.F.);
#5166=ORIENTED_EDGE('',*,*,#3789,.F.);
#5167=ORIENTED_EDGE('',*,*,#3785,.T.);
#5168=ORIENTED_EDGE('',*,*,#3783,.T.);
#5169=ORIENTED_EDGE('',*,*,#3787,.F.);
#5170=ORIENTED_EDGE('',*,*,#3781,.T.);
#5171=ORIENTED_EDGE('',*,*,#3786,.T.);
#5172=ORIENTED_EDGE('',*,*,#3789,.T.);
#5173=ORIENTED_EDGE('',*,*,#3790,.F.);
#5174=ORIENTED_EDGE('',*,*,#3791,.T.);
#5175=ORIENTED_EDGE('',*,*,#3792,.F.);
#5176=ORIENTED_EDGE('',*,*,#3791,.F.);
#5177=ORIENTED_EDGE('',*,*,#3793,.T.);
#5178=ORIENTED_EDGE('',*,*,#3794,.T.);
#5179=ORIENTED_EDGE('',*,*,#3795,.T.);
#5180=ORIENTED_EDGE('',*,*,#3796,.T.);
#5181=ORIENTED_EDGE('',*,*,#3797,.T.);
#5182=ORIENTED_EDGE('',*,*,#3790,.T.);
#5183=ORIENTED_EDGE('',*,*,#3797,.F.);
#5184=ORIENTED_EDGE('',*,*,#3798,.T.);
#5185=ORIENTED_EDGE('',*,*,#3799,.F.);
#5186=ORIENTED_EDGE('',*,*,#3798,.F.);
#5187=ORIENTED_EDGE('',*,*,#3800,.F.);
#5188=ORIENTED_EDGE('',*,*,#3801,.F.);
#5189=ORIENTED_EDGE('',*,*,#3802,.F.);
#5190=ORIENTED_EDGE('',*,*,#3796,.F.);
#5191=ORIENTED_EDGE('',*,*,#3803,.T.);
#5192=ORIENTED_EDGE('',*,*,#3804,.T.);
#5193=ORIENTED_EDGE('',*,*,#3800,.T.);
#5194=ORIENTED_EDGE('',*,*,#3795,.F.);
#5195=ORIENTED_EDGE('',*,*,#3805,.F.);
#5196=ORIENTED_EDGE('',*,*,#3806,.F.);
#5197=ORIENTED_EDGE('',*,*,#3803,.F.);
#5198=ORIENTED_EDGE('',*,*,#3794,.F.);
#5199=ORIENTED_EDGE('',*,*,#3802,.T.);
#5200=ORIENTED_EDGE('',*,*,#3807,.F.);
#5201=ORIENTED_EDGE('',*,*,#3805,.T.);
#5202=ORIENTED_EDGE('',*,*,#3793,.F.);
#5203=ORIENTED_EDGE('',*,*,#3806,.T.);
#5204=ORIENTED_EDGE('',*,*,#3807,.T.);
#5205=ORIENTED_EDGE('',*,*,#3801,.T.);
#5206=ORIENTED_EDGE('',*,*,#3804,.F.);
#5207=ORIENTED_EDGE('',*,*,#3799,.T.);
#5208=ORIENTED_EDGE('',*,*,#3792,.T.);
#5209=ORIENTED_EDGE('',*,*,#3808,.F.);
#5210=ORIENTED_EDGE('',*,*,#3809,.T.);
#5211=ORIENTED_EDGE('',*,*,#3810,.F.);
#5212=ORIENTED_EDGE('',*,*,#3809,.F.);
#5213=ORIENTED_EDGE('',*,*,#3811,.F.);
#5214=ORIENTED_EDGE('',*,*,#3812,.F.);
#5215=ORIENTED_EDGE('',*,*,#3813,.F.);
#5216=ORIENTED_EDGE('',*,*,#3814,.F.);
#5217=ORIENTED_EDGE('',*,*,#3815,.F.);
#5218=ORIENTED_EDGE('',*,*,#3816,.F.);
#5219=ORIENTED_EDGE('',*,*,#3817,.F.);
#5220=ORIENTED_EDGE('',*,*,#3818,.F.);
#5221=ORIENTED_EDGE('',*,*,#3819,.F.);
#5222=ORIENTED_EDGE('',*,*,#3820,.F.);
#5223=ORIENTED_EDGE('',*,*,#3821,.F.);
#5224=ORIENTED_EDGE('',*,*,#3822,.F.);
#5225=ORIENTED_EDGE('',*,*,#3823,.F.);
#5226=ORIENTED_EDGE('',*,*,#3812,.T.);
#5227=ORIENTED_EDGE('',*,*,#3824,.F.);
#5228=ORIENTED_EDGE('',*,*,#3825,.F.);
#5229=ORIENTED_EDGE('',*,*,#3826,.F.);
#5230=ORIENTED_EDGE('',*,*,#3827,.F.);
#5231=ORIENTED_EDGE('',*,*,#3813,.T.);
#5232=ORIENTED_EDGE('',*,*,#3823,.T.);
#5233=ORIENTED_EDGE('',*,*,#3828,.F.);
#5234=ORIENTED_EDGE('',*,*,#3829,.F.);
#5235=ORIENTED_EDGE('',*,*,#3814,.T.);
#5236=ORIENTED_EDGE('',*,*,#3827,.T.);
#5237=ORIENTED_EDGE('',*,*,#3830,.F.);
#5238=ORIENTED_EDGE('',*,*,#3831,.F.);
#5239=ORIENTED_EDGE('',*,*,#3815,.T.);
#5240=ORIENTED_EDGE('',*,*,#3829,.T.);
#5241=ORIENTED_EDGE('',*,*,#3832,.F.);
#5242=ORIENTED_EDGE('',*,*,#3833,.F.);
#5243=ORIENTED_EDGE('',*,*,#3834,.F.);
#5244=ORIENTED_EDGE('',*,*,#3835,.F.);
#5245=ORIENTED_EDGE('',*,*,#3836,.F.);
#5246=ORIENTED_EDGE('',*,*,#3816,.T.);
#5247=ORIENTED_EDGE('',*,*,#3831,.T.);
#5248=ORIENTED_EDGE('',*,*,#3837,.F.);
#5249=ORIENTED_EDGE('',*,*,#3833,.T.);
#5250=ORIENTED_EDGE('',*,*,#3838,.T.);
#5251=ORIENTED_EDGE('',*,*,#3820,.T.);
#5252=ORIENTED_EDGE('',*,*,#3839,.T.);
#5253=ORIENTED_EDGE('',*,*,#3840,.T.);
#5254=ORIENTED_EDGE('',*,*,#3810,.T.);
#5255=ORIENTED_EDGE('',*,*,#3821,.T.);
#5256=ORIENTED_EDGE('',*,*,#3838,.F.);
#5257=ORIENTED_EDGE('',*,*,#3832,.T.);
#5258=ORIENTED_EDGE('',*,*,#3841,.F.);
#5259=ORIENTED_EDGE('',*,*,#3841,.T.);
#5260=ORIENTED_EDGE('',*,*,#3837,.T.);
#5261=ORIENTED_EDGE('',*,*,#3830,.T.);
#5262=ORIENTED_EDGE('',*,*,#3828,.T.);
#5263=ORIENTED_EDGE('',*,*,#3826,.T.);
#5264=ORIENTED_EDGE('',*,*,#3822,.T.);
#5265=ORIENTED_EDGE('',*,*,#3842,.T.);
#5266=ORIENTED_EDGE('',*,*,#3808,.T.);
#5267=ORIENTED_EDGE('',*,*,#3811,.T.);
#5268=ORIENTED_EDGE('',*,*,#3836,.T.);
#5269=ORIENTED_EDGE('',*,*,#3843,.F.);
#5270=ORIENTED_EDGE('',*,*,#3824,.T.);
#5271=ORIENTED_EDGE('',*,*,#3835,.T.);
#5272=ORIENTED_EDGE('',*,*,#3844,.F.);
#5273=ORIENTED_EDGE('',*,*,#3825,.T.);
#5274=ORIENTED_EDGE('',*,*,#3843,.T.);
#5275=ORIENTED_EDGE('',*,*,#3845,.F.);
#5276=ORIENTED_EDGE('',*,*,#3846,.F.);
#5277=ORIENTED_EDGE('',*,*,#3834,.T.);
#5278=ORIENTED_EDGE('',*,*,#3839,.F.);
#5279=ORIENTED_EDGE('',*,*,#3819,.T.);
#5280=ORIENTED_EDGE('',*,*,#3844,.T.);
#5281=ORIENTED_EDGE('',*,*,#3846,.T.);
#5282=ORIENTED_EDGE('',*,*,#3847,.T.);
#5283=ORIENTED_EDGE('',*,*,#3818,.T.);
#5284=ORIENTED_EDGE('',*,*,#3847,.F.);
#5285=ORIENTED_EDGE('',*,*,#3845,.T.);
#5286=ORIENTED_EDGE('',*,*,#3848,.T.);
#5287=ORIENTED_EDGE('',*,*,#3817,.T.);
#5288=ORIENTED_EDGE('',*,*,#3848,.F.);
#5289=ORIENTED_EDGE('',*,*,#3842,.F.);
#5290=ORIENTED_EDGE('',*,*,#3849,.T.);
#5291=ORIENTED_EDGE('',*,*,#3840,.F.);
#5292=ORIENTED_EDGE('',*,*,#3849,.F.);
#5293=ORIENTED_EDGE('',*,*,#3850,.F.);
#5294=ORIENTED_EDGE('',*,*,#3851,.T.);
#5295=ORIENTED_EDGE('',*,*,#3852,.F.);
#5296=ORIENTED_EDGE('',*,*,#3851,.F.);
#5297=ORIENTED_EDGE('',*,*,#3853,.T.);
#5298=ORIENTED_EDGE('',*,*,#3854,.T.);
#5299=ORIENTED_EDGE('',*,*,#3855,.T.);
#5300=ORIENTED_EDGE('',*,*,#3856,.T.);
#5301=ORIENTED_EDGE('',*,*,#3857,.T.);
#5302=ORIENTED_EDGE('',*,*,#3850,.T.);
#5303=ORIENTED_EDGE('',*,*,#3857,.F.);
#5304=ORIENTED_EDGE('',*,*,#3858,.T.);
#5305=ORIENTED_EDGE('',*,*,#3859,.F.);
#5306=ORIENTED_EDGE('',*,*,#3858,.F.);
#5307=ORIENTED_EDGE('',*,*,#3860,.F.);
#5308=ORIENTED_EDGE('',*,*,#3861,.F.);
#5309=ORIENTED_EDGE('',*,*,#3862,.F.);
#5310=ORIENTED_EDGE('',*,*,#3856,.F.);
#5311=ORIENTED_EDGE('',*,*,#3863,.T.);
#5312=ORIENTED_EDGE('',*,*,#3864,.T.);
#5313=ORIENTED_EDGE('',*,*,#3860,.T.);
#5314=ORIENTED_EDGE('',*,*,#3855,.F.);
#5315=ORIENTED_EDGE('',*,*,#3865,.F.);
#5316=ORIENTED_EDGE('',*,*,#3866,.F.);
#5317=ORIENTED_EDGE('',*,*,#3863,.F.);
#5318=ORIENTED_EDGE('',*,*,#3854,.F.);
#5319=ORIENTED_EDGE('',*,*,#3862,.T.);
#5320=ORIENTED_EDGE('',*,*,#3867,.F.);
#5321=ORIENTED_EDGE('',*,*,#3865,.T.);
#5322=ORIENTED_EDGE('',*,*,#3853,.F.);
#5323=ORIENTED_EDGE('',*,*,#3866,.T.);
#5324=ORIENTED_EDGE('',*,*,#3867,.T.);
#5325=ORIENTED_EDGE('',*,*,#3861,.T.);
#5326=ORIENTED_EDGE('',*,*,#3864,.F.);
#5327=ORIENTED_EDGE('',*,*,#3859,.T.);
#5328=ORIENTED_EDGE('',*,*,#3852,.T.);
#5329=ORIENTED_EDGE('',*,*,#3868,.F.);
#5330=ORIENTED_EDGE('',*,*,#3869,.T.);
#5331=ORIENTED_EDGE('',*,*,#3870,.F.);
#5332=ORIENTED_EDGE('',*,*,#3869,.F.);
#5333=ORIENTED_EDGE('',*,*,#3871,.T.);
#5334=ORIENTED_EDGE('',*,*,#3872,.T.);
#5335=ORIENTED_EDGE('',*,*,#3873,.T.);
#5336=ORIENTED_EDGE('',*,*,#3874,.T.);
#5337=ORIENTED_EDGE('',*,*,#3875,.T.);
#5338=ORIENTED_EDGE('',*,*,#3868,.T.);
#5339=ORIENTED_EDGE('',*,*,#3875,.F.);
#5340=ORIENTED_EDGE('',*,*,#3876,.T.);
#5341=ORIENTED_EDGE('',*,*,#3877,.F.);
#5342=ORIENTED_EDGE('',*,*,#3876,.F.);
#5343=ORIENTED_EDGE('',*,*,#3878,.F.);
#5344=ORIENTED_EDGE('',*,*,#3879,.F.);
#5345=ORIENTED_EDGE('',*,*,#3880,.F.);
#5346=ORIENTED_EDGE('',*,*,#3874,.F.);
#5347=ORIENTED_EDGE('',*,*,#3881,.T.);
#5348=ORIENTED_EDGE('',*,*,#3882,.T.);
#5349=ORIENTED_EDGE('',*,*,#3878,.T.);
#5350=ORIENTED_EDGE('',*,*,#3873,.F.);
#5351=ORIENTED_EDGE('',*,*,#3883,.F.);
#5352=ORIENTED_EDGE('',*,*,#3884,.F.);
#5353=ORIENTED_EDGE('',*,*,#3881,.F.);
#5354=ORIENTED_EDGE('',*,*,#3872,.F.);
#5355=ORIENTED_EDGE('',*,*,#3880,.T.);
#5356=ORIENTED_EDGE('',*,*,#3885,.F.);
#5357=ORIENTED_EDGE('',*,*,#3883,.T.);
#5358=ORIENTED_EDGE('',*,*,#3871,.F.);
#5359=ORIENTED_EDGE('',*,*,#3884,.T.);
#5360=ORIENTED_EDGE('',*,*,#3885,.T.);
#5361=ORIENTED_EDGE('',*,*,#3879,.T.);
#5362=ORIENTED_EDGE('',*,*,#3882,.F.);
#5363=ORIENTED_EDGE('',*,*,#3877,.T.);
#5364=ORIENTED_EDGE('',*,*,#3870,.T.);
#5365=ORIENTED_EDGE('',*,*,#3886,.F.);
#5366=ORIENTED_EDGE('',*,*,#3887,.F.);
#5367=ORIENTED_EDGE('',*,*,#3887,.T.);
#5368=ORIENTED_EDGE('',*,*,#3886,.T.);
#5369=ORIENTED_EDGE('',*,*,#3888,.T.);
#5370=ORIENTED_EDGE('',*,*,#3889,.T.);
#5371=ORIENTED_EDGE('',*,*,#3890,.T.);
#5372=ORIENTED_EDGE('',*,*,#3888,.F.);
#5373=ORIENTED_EDGE('',*,*,#3890,.F.);
#5374=ORIENTED_EDGE('',*,*,#3889,.F.);
#5375=ORIENTED_EDGE('',*,*,#3891,.T.);
#5376=ORIENTED_EDGE('',*,*,#3892,.T.);
#5377=ORIENTED_EDGE('',*,*,#3893,.T.);
#5378=ORIENTED_EDGE('',*,*,#3892,.F.);
#5379=ORIENTED_EDGE('',*,*,#3893,.F.);
#5380=ORIENTED_EDGE('',*,*,#3891,.F.);
#5381=ORIENTED_EDGE('',*,*,#3894,.F.);
#5382=ORIENTED_EDGE('',*,*,#3895,.T.);
#5383=ORIENTED_EDGE('',*,*,#3896,.F.);
#5384=ORIENTED_EDGE('',*,*,#3895,.F.);
#5385=ORIENTED_EDGE('',*,*,#3897,.F.);
#5386=ORIENTED_EDGE('',*,*,#3896,.T.);
#5387=ORIENTED_EDGE('',*,*,#3898,.T.);
#5388=ORIENTED_EDGE('',*,*,#3894,.T.);
#5389=ORIENTED_EDGE('',*,*,#3897,.T.);
#5390=ORIENTED_EDGE('',*,*,#3899,.T.);
#5391=ORIENTED_EDGE('',*,*,#3898,.F.);
#5392=ORIENTED_EDGE('',*,*,#3899,.F.);
#5393=ORIENTED_EDGE('',*,*,#3900,.F.);
#5394=ORIENTED_EDGE('',*,*,#3901,.F.);
#5395=ORIENTED_EDGE('',*,*,#3901,.T.);
#5396=ORIENTED_EDGE('',*,*,#3902,.T.);
#5397=ORIENTED_EDGE('',*,*,#3903,.T.);
#5398=ORIENTED_EDGE('',*,*,#3904,.T.);
#5399=ORIENTED_EDGE('',*,*,#3902,.F.);
#5400=ORIENTED_EDGE('',*,*,#3900,.T.);
#5401=ORIENTED_EDGE('',*,*,#3903,.F.);
#5402=ORIENTED_EDGE('',*,*,#3904,.F.);
#5403=ORIENTED_EDGE('',*,*,#3905,.T.);
#5404=ORIENTED_EDGE('',*,*,#3906,.T.);
#5405=ORIENTED_EDGE('',*,*,#3907,.T.);
#5406=ORIENTED_EDGE('',*,*,#3906,.F.);
#5407=ORIENTED_EDGE('',*,*,#3907,.F.);
#5408=ORIENTED_EDGE('',*,*,#3905,.F.);
#5409=ORIENTED_EDGE('',*,*,#3908,.T.);
#5410=ORIENTED_EDGE('',*,*,#3909,.T.);
#5411=ORIENTED_EDGE('',*,*,#3910,.T.);
#5412=ORIENTED_EDGE('',*,*,#3909,.F.);
#5413=ORIENTED_EDGE('',*,*,#3910,.F.);
#5414=ORIENTED_EDGE('',*,*,#3911,.T.);
#5415=ORIENTED_EDGE('',*,*,#3912,.F.);
#5416=ORIENTED_EDGE('',*,*,#3913,.F.);
#5417=ORIENTED_EDGE('',*,*,#3914,.F.);
#5418=ORIENTED_EDGE('',*,*,#3915,.F.);
#5419=ORIENTED_EDGE('',*,*,#3916,.F.);
#5420=ORIENTED_EDGE('',*,*,#3917,.F.);
#5421=ORIENTED_EDGE('',*,*,#3918,.F.);
#5422=ORIENTED_EDGE('',*,*,#3919,.F.);
#5423=ORIENTED_EDGE('',*,*,#3908,.F.);
#5424=ORIENTED_EDGE('',*,*,#3920,.F.);
#5425=ORIENTED_EDGE('',*,*,#3921,.T.);
#5426=ORIENTED_EDGE('',*,*,#3911,.F.);
#5427=ORIENTED_EDGE('',*,*,#3921,.F.);
#5428=ORIENTED_EDGE('',*,*,#3922,.F.);
#5429=ORIENTED_EDGE('',*,*,#3923,.T.);
#5430=ORIENTED_EDGE('',*,*,#3919,.T.);
#5431=ORIENTED_EDGE('',*,*,#3923,.F.);
#5432=ORIENTED_EDGE('',*,*,#3924,.F.);
#5433=ORIENTED_EDGE('',*,*,#3925,.T.);
#5434=ORIENTED_EDGE('',*,*,#3918,.T.);
#5435=ORIENTED_EDGE('',*,*,#3925,.F.);
#5436=ORIENTED_EDGE('',*,*,#3926,.F.);
#5437=ORIENTED_EDGE('',*,*,#3927,.T.);
#5438=ORIENTED_EDGE('',*,*,#3917,.T.);
#5439=ORIENTED_EDGE('',*,*,#3927,.F.);
#5440=ORIENTED_EDGE('',*,*,#3928,.F.);
#5441=ORIENTED_EDGE('',*,*,#3929,.T.);
#5442=ORIENTED_EDGE('',*,*,#3916,.T.);
#5443=ORIENTED_EDGE('',*,*,#3929,.F.);
#5444=ORIENTED_EDGE('',*,*,#3930,.F.);
#5445=ORIENTED_EDGE('',*,*,#3913,.T.);
#5446=ORIENTED_EDGE('',*,*,#3931,.F.);
#5447=ORIENTED_EDGE('',*,*,#3932,.F.);
#5448=ORIENTED_EDGE('',*,*,#3914,.T.);
#5449=ORIENTED_EDGE('',*,*,#3930,.T.);
#5450=ORIENTED_EDGE('',*,*,#3933,.F.);
#5451=ORIENTED_EDGE('',*,*,#3934,.F.);
#5452=ORIENTED_EDGE('',*,*,#3935,.T.);
#5453=ORIENTED_EDGE('',*,*,#3915,.T.);
#5454=ORIENTED_EDGE('',*,*,#3934,.T.);
#5455=ORIENTED_EDGE('',*,*,#3936,.T.);
#5456=ORIENTED_EDGE('',*,*,#3912,.T.);
#5457=ORIENTED_EDGE('',*,*,#3935,.F.);
#5458=ORIENTED_EDGE('',*,*,#3937,.T.);
#5459=ORIENTED_EDGE('',*,*,#3931,.T.);
#5460=ORIENTED_EDGE('',*,*,#3932,.T.);
#5461=ORIENTED_EDGE('',*,*,#3937,.F.);
#5462=ORIENTED_EDGE('',*,*,#3936,.F.);
#5463=ORIENTED_EDGE('',*,*,#3933,.T.);
#5464=ORIENTED_EDGE('',*,*,#3928,.T.);
#5465=ORIENTED_EDGE('',*,*,#3922,.T.);
#5466=ORIENTED_EDGE('',*,*,#3924,.T.);
#5467=ORIENTED_EDGE('',*,*,#3926,.T.);
#5468=ORIENTED_EDGE('',*,*,#3920,.T.);
#5469=ORIENTED_EDGE('',*,*,#3938,.F.);
#5470=ORIENTED_EDGE('',*,*,#3939,.T.);
#5471=ORIENTED_EDGE('',*,*,#3940,.F.);
#5472=ORIENTED_EDGE('',*,*,#3939,.F.);
#5473=ORIENTED_EDGE('',*,*,#3941,.F.);
#5474=ORIENTED_EDGE('',*,*,#3940,.T.);
#5475=ORIENTED_EDGE('',*,*,#3942,.T.);
#5476=ORIENTED_EDGE('',*,*,#3938,.T.);
#5477=ORIENTED_EDGE('',*,*,#3941,.T.);
#5478=ORIENTED_EDGE('',*,*,#3943,.T.);
#5479=ORIENTED_EDGE('',*,*,#3942,.F.);
#5480=ORIENTED_EDGE('',*,*,#3943,.F.);
#5481=ORIENTED_EDGE('',*,*,#3944,.F.);
#5482=ORIENTED_EDGE('',*,*,#3945,.T.);
#5483=ORIENTED_EDGE('',*,*,#3946,.F.);
#5484=ORIENTED_EDGE('',*,*,#3945,.F.);
#5485=ORIENTED_EDGE('',*,*,#3947,.F.);
#5486=ORIENTED_EDGE('',*,*,#3946,.T.);
#5487=ORIENTED_EDGE('',*,*,#3948,.T.);
#5488=ORIENTED_EDGE('',*,*,#3944,.T.);
#5489=ORIENTED_EDGE('',*,*,#3947,.T.);
#5490=ORIENTED_EDGE('',*,*,#3949,.T.);
#5491=ORIENTED_EDGE('',*,*,#3948,.F.);
#5492=ORIENTED_EDGE('',*,*,#3949,.F.);
#5493=ORIENTED_EDGE('',*,*,#3950,.T.);
#5494=ORIENTED_EDGE('',*,*,#3951,.T.);
#5495=ORIENTED_EDGE('',*,*,#3952,.T.);
#5496=ORIENTED_EDGE('',*,*,#3951,.F.);
#5497=ORIENTED_EDGE('',*,*,#3952,.F.);
#5498=ORIENTED_EDGE('',*,*,#3950,.F.);
#5499=CYLINDRICAL_SURFACE('',#6409,0.00749999975240882);
#5500=CYLINDRICAL_SURFACE('',#6412,0.042);
#5501=CYLINDRICAL_SURFACE('',#6421,0.05);
#5502=CYLINDRICAL_SURFACE('',#6423,0.05);
#5503=CYLINDRICAL_SURFACE('',#6429,0.04);
#5504=CYLINDRICAL_SURFACE('',#6431,0.04);
#5505=CYLINDRICAL_SURFACE('',#6449,0.028);
#5506=CYLINDRICAL_SURFACE('',#6451,0.0025);
#5507=CYLINDRICAL_SURFACE('',#6452,0.0025);
#5508=CYLINDRICAL_SURFACE('',#6453,0.0025);
#5509=CYLINDRICAL_SURFACE('',#6454,0.0025);
#5510=CYLINDRICAL_SURFACE('',#6455,0.0025);
#5511=CYLINDRICAL_SURFACE('',#6456,0.0025);
#5512=CYLINDRICAL_SURFACE('',#6457,0.028);
#5513=CYLINDRICAL_SURFACE('',#6470,0.026);
#5514=CYLINDRICAL_SURFACE('',#6479,0.02045);
#5515=CYLINDRICAL_SURFACE('',#6490,0.02045);
#5516=CYLINDRICAL_SURFACE('',#6493,0.01305);
#5517=CYLINDRICAL_SURFACE('',#6502,0.01305);
#5518=CYLINDRICAL_SURFACE('',#6513,0.0075);
#5519=CYLINDRICAL_SURFACE('',#6529,0.026);
#5520=CYLINDRICAL_SURFACE('',#6538,0.02045);
#5521=CYLINDRICAL_SURFACE('',#6549,0.02045);
#5522=CYLINDRICAL_SURFACE('',#6552,0.01305);
#5523=CYLINDRICAL_SURFACE('',#6561,0.01305);
#5524=CYLINDRICAL_SURFACE('',#6572,0.0075);
#5525=CYLINDRICAL_SURFACE('',#6580,0.042);
#5526=CYLINDRICAL_SURFACE('',#6589,0.05);
#5527=CYLINDRICAL_SURFACE('',#6591,0.05);
#5528=CYLINDRICAL_SURFACE('',#6597,0.04);
#5529=CYLINDRICAL_SURFACE('',#6599,0.04);
#5530=CYLINDRICAL_SURFACE('',#6617,0.028);
#5531=CYLINDRICAL_SURFACE('',#6619,0.0025);
#5532=CYLINDRICAL_SURFACE('',#6620,0.0025);
#5533=CYLINDRICAL_SURFACE('',#6621,0.0025);
#5534=CYLINDRICAL_SURFACE('',#6622,0.0025);
#5535=CYLINDRICAL_SURFACE('',#6623,0.0025);
#5536=CYLINDRICAL_SURFACE('',#6624,0.0025);
#5537=CYLINDRICAL_SURFACE('',#6625,0.028);
#5538=CYLINDRICAL_SURFACE('',#6631,0.025);
#5539=CYLINDRICAL_SURFACE('',#6633,0.042);
#5540=CYLINDRICAL_SURFACE('',#6642,0.042);
#5541=CYLINDRICAL_SURFACE('',#6646,0.05);
#5542=CYLINDRICAL_SURFACE('',#6656,0.05);
#5543=CYLINDRICAL_SURFACE('',#6658,0.005);
#5544=CYLINDRICAL_SURFACE('',#6671,0.005);
#5545=CYLINDRICAL_SURFACE('',#6672,0.005);
#5546=CYLINDRICAL_SURFACE('',#6673,0.025);
#5547=CYLINDRICAL_SURFACE('',#6674,0.005);
#5548=CYLINDRICAL_SURFACE('',#6688,0.026);
#5549=CYLINDRICAL_SURFACE('',#6697,0.02045);
#5550=CYLINDRICAL_SURFACE('',#6708,0.02045);
#5551=CYLINDRICAL_SURFACE('',#6711,0.01305);
#5552=CYLINDRICAL_SURFACE('',#6720,0.01305);
#5553=CYLINDRICAL_SURFACE('',#6731,0.0075);
#5554=CYLINDRICAL_SURFACE('',#6739,0.028);
#5555=CYLINDRICAL_SURFACE('',#6751,0.025);
#5556=CYLINDRICAL_SURFACE('',#6753,0.0049999999999998);
#5557=CYLINDRICAL_SURFACE('',#6755,0.005);
#5558=CYLINDRICAL_SURFACE('',#6757,0.0049999999999998);
#5559=CYLINDRICAL_SURFACE('',#6759,0.005);
#5560=CYLINDRICAL_SURFACE('',#6763,0.05);
#5561=CYLINDRICAL_SURFACE('',#6765,0.299);
#5562=CYLINDRICAL_SURFACE('',#6777,0.026);
#5563=CYLINDRICAL_SURFACE('',#6786,0.02045);
#5564=CYLINDRICAL_SURFACE('',#6797,0.02045);
#5565=CYLINDRICAL_SURFACE('',#6800,0.01305);
#5566=CYLINDRICAL_SURFACE('',#6809,0.01305);
#5567=CYLINDRICAL_SURFACE('',#6820,0.0075);
#5568=CYLINDRICAL_SURFACE('',#6829,0.00799999973819874);
#5569=CYLINDRICAL_SURFACE('',#6835,0.00999999988959839);
#5570=CYLINDRICAL_SURFACE('',#6839,0.00799999961340774);
#5571=CYLINDRICAL_SURFACE('',#6861,0.00799999959059736);
#5572=CYLINDRICAL_SURFACE('',#6867,0.0099999996557502);
#5573=CYLINDRICAL_SURFACE('',#6871,0.00799999974118007);
#5574=CYLINDRICAL_SURFACE('',#6893,0.0079999999576051);
#5575=CYLINDRICAL_SURFACE('',#6915,0.00799999974106502);
#5576=CYLINDRICAL_SURFACE('',#6921,0.00999999987547767);
#5577=CYLINDRICAL_SURFACE('',#6925,0.00749999975240883);
#5578=CYLINDRICAL_SURFACE('',#6930,0.00749999975240883);
#5579=CYLINDRICAL_SURFACE('',#6934,0.00749999975240883);
#5580=CYLINDRICAL_SURFACE('',#6938,0.00749999975240883);
#5581=CYLINDRICAL_SURFACE('',#6941,0.00749999975240883);
#5582=CYLINDRICAL_SURFACE('',#6946,0.0075);
#5583=CYLINDRICAL_SURFACE('',#6947,0.015);
#5584=CYLINDRICAL_SURFACE('',#6949,0.0075);
#5585=CYLINDRICAL_SURFACE('',#6951,0.0075);
#5586=CYLINDRICAL_SURFACE('',#6962,0.01);
#5587=CYLINDRICAL_SURFACE('',#6983,0.00499999999997557);
#5588=CYLINDRICAL_SURFACE('',#6984,0.00499999999997558);
#5589=CYLINDRICAL_SURFACE('',#6985,0.00500000000000013);
#5590=CYLINDRICAL_SURFACE('',#6986,0.005);
#5591=CYLINDRICAL_SURFACE('',#6987,0.005);
#5592=CYLINDRICAL_SURFACE('',#6988,0.00500000000000013);
#5593=CYLINDRICAL_SURFACE('',#6989,0.00499999999997557);
#5594=CYLINDRICAL_SURFACE('',#6990,0.00499999999997558);
#5595=CYLINDRICAL_SURFACE('',#7021,0.005);
#5596=CYLINDRICAL_SURFACE('',#7022,0.005);
#5597=CYLINDRICAL_SURFACE('',#7023,0.00500000000000013);
#5598=CYLINDRICAL_SURFACE('',#7024,0.005);
#5599=CYLINDRICAL_SURFACE('',#7025,0.005);
#5600=CYLINDRICAL_SURFACE('',#7026,0.00500000000000013);
#5601=CYLINDRICAL_SURFACE('',#7027,0.005);
#5602=CYLINDRICAL_SURFACE('',#7028,0.005);
#5603=CYLINDRICAL_SURFACE('',#7029,0.01);
#5604=CYLINDRICAL_SURFACE('',#7031,0.003);
#5605=CYLINDRICAL_SURFACE('',#7037,0.0125);
#5606=CYLINDRICAL_SURFACE('',#7041,0.003);
#5607=CYLINDRICAL_SURFACE('',#7046,0.00118970000000007);
#5608=CYLINDRICAL_SURFACE('',#7052,0.00118970100000004);
#5609=CYLINDRICAL_SURFACE('',#7055,0.007216878);
#5610=CYLINDRICAL_SURFACE('',#7068,0.00118970000000007);
#5611=CYLINDRICAL_SURFACE('',#7074,0.00118970100000004);
#5612=CYLINDRICAL_SURFACE('',#7077,0.007216878);
#5613=CYLINDRICAL_SURFACE('',#7083,0.00118970099999992);
#5614=CYLINDRICAL_SURFACE('',#7104,0.00118970100010167);
#5615=CYLINDRICAL_SURFACE('',#7105,0.00118970100010167);
#5616=CYLINDRICAL_SURFACE('',#7106,0.00118970099999992);
#5617=CYLINDRICAL_SURFACE('',#7108,0.00118970000000007);
#5618=CYLINDRICAL_SURFACE('',#7114,0.00118970100000004);
#5619=CYLINDRICAL_SURFACE('',#7117,0.007216878);
#5620=CYLINDRICAL_SURFACE('',#7123,0.00118970000000007);
#5621=CYLINDRICAL_SURFACE('',#7129,0.00118970100000004);
#5622=CYLINDRICAL_SURFACE('',#7132,0.007216878);
#5623=CYLINDRICAL_SURFACE('',#7145,0.0250000000000019);
#5624=CYLINDRICAL_SURFACE('',#7148,0.0249999998982604);
#5625=CYLINDRICAL_SURFACE('',#7151,0.025);
#5626=CYLINDRICAL_SURFACE('',#7153,0.025);
#5627=CYLINDRICAL_SURFACE('',#7159,0.025);
#5628=CYLINDRICAL_SURFACE('',#7166,0.035);
#5629=CYLINDRICAL_SURFACE('',#7168,0.0250000000000019);
#5630=CYLINDRICAL_SURFACE('',#7171,0.0249999998982604);
#5631=CYLINDRICAL_SURFACE('',#7174,0.025);
#5632=CYLINDRICAL_SURFACE('',#7176,0.025);
#5633=CYLINDRICAL_SURFACE('',#7187,0.028);
#5634=CYLINDRICAL_SURFACE('',#7199,0.025);
#5635=CYLINDRICAL_SURFACE('',#7201,0.0049999999999998);
#5636=CYLINDRICAL_SURFACE('',#7203,0.005);
#5637=CYLINDRICAL_SURFACE('',#7205,0.0049999999999998);
#5638=CYLINDRICAL_SURFACE('',#7207,0.005);
#5639=CYLINDRICAL_SURFACE('',#7210,0.299);
#5640=CYLINDRICAL_SURFACE('',#7212,0.05);
#5641=CYLINDRICAL_SURFACE('',#7218,0.025);
#5642=CYLINDRICAL_SURFACE('',#7225,0.174999999);
#5643=CYLINDRICAL_SURFACE('',#7227,0.025);
#5644=CYLINDRICAL_SURFACE('',#7234,0.174999999);
#5645=CYLINDRICAL_SURFACE('',#7236,0.025);
#5646=ADVANCED_FACE('',(#673),#5499,.F.);
#5647=ADVANCED_FACE('',(#674),#5500,.T.);
#5648=ADVANCED_FACE('',(#675),#665,.T.);
#5649=ADVANCED_FACE('',(#676),#666,.T.);
#5650=ADVANCED_FACE('',(#677),#5501,.T.);
#5651=ADVANCED_FACE('',(#678),#5502,.T.);
#5652=ADVANCED_FACE('',(#679,#339),#496,.F.);
#5653=ADVANCED_FACE('',(#680,#340),#497,.T.);
#5654=ADVANCED_FACE('',(#681),#5503,.F.);
#5655=ADVANCED_FACE('',(#682),#5504,.F.);
#5656=ADVANCED_FACE('',(#683,#341,#342,#343,#344,#345,#346,#347),#498,.F.);
#5657=ADVANCED_FACE('',(#684,#348,#349,#350,#351,#352,#353,#354),#499,.T.);
#5658=ADVANCED_FACE('',(#685),#5505,.T.);
#5659=ADVANCED_FACE('',(#686),#5506,.F.);
#5660=ADVANCED_FACE('',(#687),#5507,.F.);
#5661=ADVANCED_FACE('',(#688),#5508,.F.);
#5662=ADVANCED_FACE('',(#689),#5509,.F.);
#5663=ADVANCED_FACE('',(#690),#5510,.F.);
#5664=ADVANCED_FACE('',(#691),#5511,.F.);
#5665=ADVANCED_FACE('',(#692),#5512,.T.);
#5666=ADVANCED_FACE('',(#693,#355),#500,.F.);
#5667=ADVANCED_FACE('',(#694,#356),#501,.T.);
#5668=ADVANCED_FACE('',(#695),#167,.T.);
#5669=ADVANCED_FACE('',(#696),#168,.T.);
#5670=ADVANCED_FACE('',(#697),#5513,.T.);
#5671=ADVANCED_FACE('',(#698,#357),#502,.T.);
#5672=ADVANCED_FACE('',(#699),#169,.T.);
#5673=ADVANCED_FACE('',(#700),#5514,.F.);
#5674=ADVANCED_FACE('',(#701),#170,.T.);
#5675=ADVANCED_FACE('',(#702,#358),#503,.T.);
#5676=ADVANCED_FACE('',(#703),#171,.T.);
#5677=ADVANCED_FACE('',(#704),#5515,.F.);
#5678=ADVANCED_FACE('',(#705),#5516,.T.);
#5679=ADVANCED_FACE('',(#706),#172,.T.);
#5680=ADVANCED_FACE('',(#707,#359),#504,.T.);
#5681=ADVANCED_FACE('',(#708),#5517,.T.);
#5682=ADVANCED_FACE('',(#709),#173,.T.);
#5683=ADVANCED_FACE('',(#710),#174,.T.);
#5684=ADVANCED_FACE('',(#711,#360),#505,.T.);
#5685=ADVANCED_FACE('',(#712),#5518,.F.);
#5686=ADVANCED_FACE('',(#713),#175,.T.);
#5687=ADVANCED_FACE('',(#714),#176,.T.);
#5688=ADVANCED_FACE('',(#715),#177,.T.);
#5689=ADVANCED_FACE('',(#716),#178,.T.);
#5690=ADVANCED_FACE('',(#717),#5519,.T.);
#5691=ADVANCED_FACE('',(#718,#361),#506,.T.);
#5692=ADVANCED_FACE('',(#719),#179,.T.);
#5693=ADVANCED_FACE('',(#720),#5520,.F.);
#5694=ADVANCED_FACE('',(#721),#180,.T.);
#5695=ADVANCED_FACE('',(#722,#362),#507,.T.);
#5696=ADVANCED_FACE('',(#723),#181,.T.);
#5697=ADVANCED_FACE('',(#724),#5521,.F.);
#5698=ADVANCED_FACE('',(#725),#5522,.T.);
#5699=ADVANCED_FACE('',(#726),#182,.T.);
#5700=ADVANCED_FACE('',(#727,#363),#508,.T.);
#5701=ADVANCED_FACE('',(#728),#5523,.T.);
#5702=ADVANCED_FACE('',(#729),#183,.T.);
#5703=ADVANCED_FACE('',(#730),#184,.T.);
#5704=ADVANCED_FACE('',(#731,#364),#509,.T.);
#5705=ADVANCED_FACE('',(#732),#5524,.F.);
#5706=ADVANCED_FACE('',(#733),#185,.T.);
#5707=ADVANCED_FACE('',(#734),#186,.T.);
#5708=ADVANCED_FACE('',(#735),#5525,.T.);
#5709=ADVANCED_FACE('',(#736),#667,.T.);
#5710=ADVANCED_FACE('',(#737),#668,.T.);
#5711=ADVANCED_FACE('',(#738),#5526,.T.);
#5712=ADVANCED_FACE('',(#739),#5527,.T.);
#5713=ADVANCED_FACE('',(#740,#365),#510,.F.);
#5714=ADVANCED_FACE('',(#741,#366),#511,.T.);
#5715=ADVANCED_FACE('',(#742),#5528,.F.);
#5716=ADVANCED_FACE('',(#743),#5529,.F.);
#5717=ADVANCED_FACE('',(#744,#367,#368,#369,#370,#371,#372,#373),#512,.F.);
#5718=ADVANCED_FACE('',(#745,#374,#375,#376,#377,#378,#379,#380),#513,.T.);
#5719=ADVANCED_FACE('',(#746),#5530,.T.);
#5720=ADVANCED_FACE('',(#747),#5531,.F.);
#5721=ADVANCED_FACE('',(#748),#5532,.F.);
#5722=ADVANCED_FACE('',(#749),#5533,.F.);
#5723=ADVANCED_FACE('',(#750),#5534,.F.);
#5724=ADVANCED_FACE('',(#751),#5535,.F.);
#5725=ADVANCED_FACE('',(#752),#5536,.F.);
#5726=ADVANCED_FACE('',(#753),#5537,.T.);
#5727=ADVANCED_FACE('',(#754,#381),#514,.F.);
#5728=ADVANCED_FACE('',(#755,#382),#515,.T.);
#5729=ADVANCED_FACE('',(#756),#5538,.F.);
#5730=ADVANCED_FACE('',(#757),#5539,.F.);
#5731=ADVANCED_FACE('',(#758),#516,.F.);
#5732=ADVANCED_FACE('',(#759),#669,.F.);
#5733=ADVANCED_FACE('',(#760),#670,.F.);
#5734=ADVANCED_FACE('',(#761),#517,.F.);
#5735=ADVANCED_FACE('',(#762),#5540,.F.);
#5736=ADVANCED_FACE('',(#763),#518,.F.);
#5737=ADVANCED_FACE('',(#764),#5541,.T.);
#5738=ADVANCED_FACE('',(#765),#519,.F.);
#5739=ADVANCED_FACE('',(#766),#520,.F.);
#5740=ADVANCED_FACE('',(#767),#521,.F.);
#5741=ADVANCED_FACE('',(#768),#671,.F.);
#5742=ADVANCED_FACE('',(#769),#672,.F.);
#5743=ADVANCED_FACE('',(#770),#522,.F.);
#5744=ADVANCED_FACE('',(#771),#523,.F.);
#5745=ADVANCED_FACE('',(#772),#5542,.T.);
#5746=ADVANCED_FACE('',(#773),#5543,.F.);
#5747=ADVANCED_FACE('',(#774,#383,#384,#385,#386,#387),#524,.F.);
#5748=ADVANCED_FACE('',(#775,#388,#389,#390,#391,#392),#525,.T.);
#5749=ADVANCED_FACE('',(#776),#5544,.F.);
#5750=ADVANCED_FACE('',(#777),#5545,.F.);
#5751=ADVANCED_FACE('',(#778),#5546,.F.);
#5752=ADVANCED_FACE('',(#779),#5547,.F.);
#5753=ADVANCED_FACE('',(#780),#526,.F.);
#5754=ADVANCED_FACE('',(#781),#527,.T.);
#5755=ADVANCED_FACE('',(#782),#528,.T.);
#5756=ADVANCED_FACE('',(#783),#529,.F.);
#5757=ADVANCED_FACE('',(#784),#187,.T.);
#5758=ADVANCED_FACE('',(#785),#188,.T.);
#5759=ADVANCED_FACE('',(#786),#5548,.T.);
#5760=ADVANCED_FACE('',(#787,#393),#530,.T.);
#5761=ADVANCED_FACE('',(#788),#189,.T.);
#5762=ADVANCED_FACE('',(#789),#5549,.F.);
#5763=ADVANCED_FACE('',(#790),#190,.T.);
#5764=ADVANCED_FACE('',(#791,#394),#531,.T.);
#5765=ADVANCED_FACE('',(#792),#191,.T.);
#5766=ADVANCED_FACE('',(#793),#5550,.F.);
#5767=ADVANCED_FACE('',(#794),#5551,.T.);
#5768=ADVANCED_FACE('',(#795),#192,.T.);
#5769=ADVANCED_FACE('',(#796,#395),#532,.T.);
#5770=ADVANCED_FACE('',(#797),#5552,.T.);
#5771=ADVANCED_FACE('',(#798),#193,.T.);
#5772=ADVANCED_FACE('',(#799),#194,.T.);
#5773=ADVANCED_FACE('',(#800,#396),#533,.T.);
#5774=ADVANCED_FACE('',(#801),#5553,.F.);
#5775=ADVANCED_FACE('',(#802),#195,.T.);
#5776=ADVANCED_FACE('',(#803),#196,.T.);
#5777=ADVANCED_FACE('',(#804),#5554,.T.);
#5778=ADVANCED_FACE('',(#805,#397),#534,.T.);
#5779=ADVANCED_FACE('',(#806,#398,#399,#400,#401,#402),#535,.F.);
#5780=ADVANCED_FACE('',(#807),#5555,.F.);
#5781=ADVANCED_FACE('',(#808),#5556,.F.);
#5782=ADVANCED_FACE('',(#809),#5557,.F.);
#5783=ADVANCED_FACE('',(#810),#5558,.F.);
#5784=ADVANCED_FACE('',(#811),#5559,.F.);
#5785=ADVANCED_FACE('',(#812),#536,.F.);
#5786=ADVANCED_FACE('',(#813),#537,.T.);
#5787=ADVANCED_FACE('',(#814),#5560,.T.);
#5788=ADVANCED_FACE('',(#815),#5561,.F.);
#5789=ADVANCED_FACE('',(#816,#403,#404,#405,#406,#407),#538,.T.);
#5790=ADVANCED_FACE('',(#817),#197,.T.);
#5791=ADVANCED_FACE('',(#818),#198,.T.);
#5792=ADVANCED_FACE('',(#819),#5562,.T.);
#5793=ADVANCED_FACE('',(#820,#408),#539,.T.);
#5794=ADVANCED_FACE('',(#821),#199,.T.);
#5795=ADVANCED_FACE('',(#822),#5563,.F.);
#5796=ADVANCED_FACE('',(#823),#200,.T.);
#5797=ADVANCED_FACE('',(#824,#409),#540,.T.);
#5798=ADVANCED_FACE('',(#825),#201,.T.);
#5799=ADVANCED_FACE('',(#826),#5564,.F.);
#5800=ADVANCED_FACE('',(#827),#5565,.T.);
#5801=ADVANCED_FACE('',(#828),#202,.T.);
#5802=ADVANCED_FACE('',(#829,#410),#541,.T.);
#5803=ADVANCED_FACE('',(#830),#5566,.T.);
#5804=ADVANCED_FACE('',(#831),#203,.T.);
#5805=ADVANCED_FACE('',(#832),#204,.T.);
#5806=ADVANCED_FACE('',(#833,#411),#542,.T.);
#5807=ADVANCED_FACE('',(#834),#5567,.F.);
#5808=ADVANCED_FACE('',(#835),#205,.T.);
#5809=ADVANCED_FACE('',(#836),#206,.T.);
#5810=ADVANCED_FACE('',(#837),#5568,.F.);
#5811=ADVANCED_FACE('',(#838),#543,.F.);
#5812=ADVANCED_FACE('',(#839,#412),#544,.F.);
#5813=ADVANCED_FACE('',(#840),#5569,.T.);
#5814=ADVANCED_FACE('',(#841),#545,.T.);
#5815=ADVANCED_FACE('',(#842),#5570,.T.);
#5816=ADVANCED_FACE('',(#843),#546,.F.);
#5817=ADVANCED_FACE('',(#844),#547,.T.);
#5818=ADVANCED_FACE('',(#845),#548,.T.);
#5819=ADVANCED_FACE('',(#846),#549,.T.);
#5820=ADVANCED_FACE('',(#847),#550,.T.);
#5821=ADVANCED_FACE('',(#848),#551,.T.);
#5822=ADVANCED_FACE('',(#849),#552,.T.);
#5823=ADVANCED_FACE('',(#850),#553,.F.);
#5824=ADVANCED_FACE('',(#851),#554,.F.);
#5825=ADVANCED_FACE('',(#852),#555,.T.);
#5826=ADVANCED_FACE('',(#853),#556,.T.);
#5827=ADVANCED_FACE('',(#854),#557,.F.);
#5828=ADVANCED_FACE('',(#855),#5571,.F.);
#5829=ADVANCED_FACE('',(#856),#558,.F.);
#5830=ADVANCED_FACE('',(#857,#413),#559,.F.);
#5831=ADVANCED_FACE('',(#858),#5572,.T.);
#5832=ADVANCED_FACE('',(#859),#560,.T.);
#5833=ADVANCED_FACE('',(#860),#5573,.T.);
#5834=ADVANCED_FACE('',(#861),#561,.F.);
#5835=ADVANCED_FACE('',(#862),#562,.T.);
#5836=ADVANCED_FACE('',(#863),#563,.T.);
#5837=ADVANCED_FACE('',(#864),#564,.T.);
#5838=ADVANCED_FACE('',(#865),#565,.T.);
#5839=ADVANCED_FACE('',(#866),#566,.T.);
#5840=ADVANCED_FACE('',(#867),#567,.T.);
#5841=ADVANCED_FACE('',(#868),#568,.F.);
#5842=ADVANCED_FACE('',(#869),#569,.F.);
#5843=ADVANCED_FACE('',(#870),#570,.T.);
#5844=ADVANCED_FACE('',(#871),#571,.T.);
#5845=ADVANCED_FACE('',(#872),#572,.F.);
#5846=ADVANCED_FACE('',(#873),#5574,.T.);
#5847=ADVANCED_FACE('',(#874),#573,.F.);
#5848=ADVANCED_FACE('',(#875),#574,.T.);
#5849=ADVANCED_FACE('',(#876),#575,.T.);
#5850=ADVANCED_FACE('',(#877),#576,.T.);
#5851=ADVANCED_FACE('',(#878),#577,.T.);
#5852=ADVANCED_FACE('',(#879),#578,.T.);
#5853=ADVANCED_FACE('',(#880),#579,.T.);
#5854=ADVANCED_FACE('',(#881),#580,.F.);
#5855=ADVANCED_FACE('',(#882),#581,.F.);
#5856=ADVANCED_FACE('',(#883),#582,.T.);
#5857=ADVANCED_FACE('',(#884),#583,.T.);
#5858=ADVANCED_FACE('',(#885),#584,.F.);
#5859=ADVANCED_FACE('',(#886),#5575,.F.);
#5860=ADVANCED_FACE('',(#887),#585,.F.);
#5861=ADVANCED_FACE('',(#888,#414),#586,.F.);
#5862=ADVANCED_FACE('',(#889),#5576,.T.);
#5863=ADVANCED_FACE('',(#890),#587,.T.);
#5864=ADVANCED_FACE('',(#891),#5577,.T.);
#5865=ADVANCED_FACE('',(#892),#5578,.T.);
#5866=ADVANCED_FACE('',(#893),#5579,.T.);
#5867=ADVANCED_FACE('',(#894),#5580,.T.);
#5868=ADVANCED_FACE('',(#895),#5581,.T.);
#5869=ADVANCED_FACE('',(#896,#415),#588,.F.);
#5870=ADVANCED_FACE('',(#897),#5582,.T.);
#5871=ADVANCED_FACE('',(#898),#5583,.T.);
#5872=ADVANCED_FACE('',(#899),#5584,.T.);
#5873=ADVANCED_FACE('',(#900,#416),#589,.F.);
#5874=ADVANCED_FACE('',(#901),#5585,.T.);
#5875=ADVANCED_FACE('',(#902),#590,.T.);
#5876=ADVANCED_FACE('',(#903),#591,.T.);
#5877=ADVANCED_FACE('',(#904),#5586,.F.);
#5878=ADVANCED_FACE('',(#905,#417,#418,#419,#420,#421,#422,#423,#424,#425),
#592,.F.);
#5879=ADVANCED_FACE('',(#906,#426,#427,#428,#429,#430,#431,#432,#433,#434),
#593,.T.);
#5880=ADVANCED_FACE('',(#907),#5587,.F.);
#5881=ADVANCED_FACE('',(#908),#5588,.F.);
#5882=ADVANCED_FACE('',(#909),#5589,.F.);
#5883=ADVANCED_FACE('',(#910),#5590,.F.);
#5884=ADVANCED_FACE('',(#911),#5591,.F.);
#5885=ADVANCED_FACE('',(#912),#5592,.F.);
#5886=ADVANCED_FACE('',(#913),#5593,.F.);
#5887=ADVANCED_FACE('',(#914),#5594,.F.);
#5888=ADVANCED_FACE('',(#915),#594,.F.);
#5889=ADVANCED_FACE('',(#916),#595,.F.);
#5890=ADVANCED_FACE('',(#917),#596,.F.);
#5891=ADVANCED_FACE('',(#918),#597,.F.);
#5892=ADVANCED_FACE('',(#919),#598,.F.);
#5893=ADVANCED_FACE('',(#920),#599,.T.);
#5894=ADVANCED_FACE('',(#921),#600,.T.);
#5895=ADVANCED_FACE('',(#922),#601,.T.);
#5896=ADVANCED_FACE('',(#923),#602,.F.);
#5897=ADVANCED_FACE('',(#924,#435,#436,#437,#438,#439,#440,#441,#442,#443),
#603,.F.);
#5898=ADVANCED_FACE('',(#925,#444,#445,#446,#447,#448,#449,#450,#451,#452),
#604,.T.);
#5899=ADVANCED_FACE('',(#926),#605,.F.);
#5900=ADVANCED_FACE('',(#927),#5595,.F.);
#5901=ADVANCED_FACE('',(#928),#5596,.F.);
#5902=ADVANCED_FACE('',(#929),#5597,.F.);
#5903=ADVANCED_FACE('',(#930),#5598,.F.);
#5904=ADVANCED_FACE('',(#931),#5599,.F.);
#5905=ADVANCED_FACE('',(#932),#5600,.F.);
#5906=ADVANCED_FACE('',(#933),#5601,.F.);
#5907=ADVANCED_FACE('',(#934),#5602,.F.);
#5908=ADVANCED_FACE('',(#935),#5603,.F.);
#5909=ADVANCED_FACE('',(#936),#5604,.T.);
#5910=ADVANCED_FACE('',(#937),#606,.T.);
#5911=ADVANCED_FACE('',(#938,#453),#607,.T.);
#5912=ADVANCED_FACE('',(#939),#5605,.T.);
#5913=ADVANCED_FACE('',(#940,#454),#608,.F.);
#5914=ADVANCED_FACE('',(#941),#5606,.T.);
#5915=ADVANCED_FACE('',(#942),#609,.F.);
#5916=ADVANCED_FACE('',(#943),#5607,.F.);
#5917=ADVANCED_FACE('',(#944,#455,#456),#610,.T.);
#5918=ADVANCED_FACE('',(#945),#5608,.F.);
#5919=ADVANCED_FACE('',(#946),#611,.F.);
#5920=ADVANCED_FACE('',(#947),#5609,.T.);
#5921=ADVANCED_FACE('',(#948),#612,.F.);
#5922=ADVANCED_FACE('',(#949),#613,.F.);
#5923=ADVANCED_FACE('',(#950,#457,#458),#614,.F.);
#5924=ADVANCED_FACE('',(#951),#615,.F.);
#5925=ADVANCED_FACE('',(#952),#616,.F.);
#5926=ADVANCED_FACE('',(#953),#617,.F.);
#5927=ADVANCED_FACE('',(#954),#618,.T.);
#5928=ADVANCED_FACE('',(#955),#619,.F.);
#5929=ADVANCED_FACE('',(#956),#620,.F.);
#5930=ADVANCED_FACE('',(#957),#5610,.F.);
#5931=ADVANCED_FACE('',(#958,#459,#460),#621,.T.);
#5932=ADVANCED_FACE('',(#959),#5611,.F.);
#5933=ADVANCED_FACE('',(#960),#622,.F.);
#5934=ADVANCED_FACE('',(#961),#5612,.T.);
#5935=ADVANCED_FACE('',(#962),#623,.F.);
#5936=ADVANCED_FACE('',(#963),#624,.F.);
#5937=ADVANCED_FACE('',(#964,#461,#462),#625,.F.);
#5938=ADVANCED_FACE('',(#965),#5613,.F.);
#5939=ADVANCED_FACE('',(#966,#463,#464),#626,.F.);
#5940=ADVANCED_FACE('',(#967),#627,.F.);
#5941=ADVANCED_FACE('',(#968),#628,.F.);
#5942=ADVANCED_FACE('',(#969),#629,.F.);
#5943=ADVANCED_FACE('',(#970),#630,.F.);
#5944=ADVANCED_FACE('',(#971),#631,.F.);
#5945=ADVANCED_FACE('',(#972,#465,#466),#632,.T.);
#5946=ADVANCED_FACE('',(#973),#633,.F.);
#5947=ADVANCED_FACE('',(#974,#467,#468),#634,.T.);
#5948=ADVANCED_FACE('',(#975),#635,.F.);
#5949=ADVANCED_FACE('',(#976,#469,#470),#636,.F.);
#5950=ADVANCED_FACE('',(#977),#637,.F.);
#5951=ADVANCED_FACE('',(#978),#5614,.F.);
#5952=ADVANCED_FACE('',(#979),#5615,.F.);
#5953=ADVANCED_FACE('',(#980),#5616,.F.);
#5954=ADVANCED_FACE('',(#981),#5617,.F.);
#5955=ADVANCED_FACE('',(#982,#471,#472),#638,.T.);
#5956=ADVANCED_FACE('',(#983),#5618,.F.);
#5957=ADVANCED_FACE('',(#984),#639,.F.);
#5958=ADVANCED_FACE('',(#985),#5619,.T.);
#5959=ADVANCED_FACE('',(#986),#640,.F.);
#5960=ADVANCED_FACE('',(#987),#641,.F.);
#5961=ADVANCED_FACE('',(#988,#473,#474),#642,.F.);
#5962=ADVANCED_FACE('',(#989),#5620,.F.);
#5963=ADVANCED_FACE('',(#990,#475,#476),#643,.T.);
#5964=ADVANCED_FACE('',(#991),#5621,.F.);
#5965=ADVANCED_FACE('',(#992),#644,.F.);
#5966=ADVANCED_FACE('',(#993),#5622,.T.);
#5967=ADVANCED_FACE('',(#994),#645,.F.);
#5968=ADVANCED_FACE('',(#995),#646,.F.);
#5969=ADVANCED_FACE('',(#996,#477,#478),#647,.F.);
#5970=ADVANCED_FACE('',(#997),#5623,.F.);
#5971=ADVANCED_FACE('',(#998),#5624,.T.);
#5972=ADVANCED_FACE('',(#999),#5625,.F.);
#5973=ADVANCED_FACE('',(#1000),#5626,.T.);
#5974=ADVANCED_FACE('',(#1001),#648,.T.);
#5975=ADVANCED_FACE('',(#1002),#649,.F.);
#5976=ADVANCED_FACE('',(#1003),#5627,.F.);
#5977=ADVANCED_FACE('',(#1004,#479),#650,.F.);
#5978=ADVANCED_FACE('',(#1005,#480),#651,.T.);
#5979=ADVANCED_FACE('',(#1006),#5628,.T.);
#5980=ADVANCED_FACE('',(#1007),#5629,.F.);
#5981=ADVANCED_FACE('',(#1008),#5630,.T.);
#5982=ADVANCED_FACE('',(#1009),#5631,.F.);
#5983=ADVANCED_FACE('',(#1010),#5632,.T.);
#5984=ADVANCED_FACE('',(#1011),#652,.T.);
#5985=ADVANCED_FACE('',(#1012),#653,.F.);
#5986=ADVANCED_FACE('',(#1013),#5633,.T.);
#5987=ADVANCED_FACE('',(#1014,#481),#654,.T.);
#5988=ADVANCED_FACE('',(#1015,#482,#483,#484,#485,#486),#655,.F.);
#5989=ADVANCED_FACE('',(#1016),#5634,.F.);
#5990=ADVANCED_FACE('',(#1017),#5635,.F.);
#5991=ADVANCED_FACE('',(#1018),#5636,.F.);
#5992=ADVANCED_FACE('',(#1019),#5637,.F.);
#5993=ADVANCED_FACE('',(#1020),#5638,.F.);
#5994=ADVANCED_FACE('',(#1021),#656,.F.);
#5995=ADVANCED_FACE('',(#1022),#5639,.F.);
#5996=ADVANCED_FACE('',(#1023),#5640,.T.);
#5997=ADVANCED_FACE('',(#1024),#657,.T.);
#5998=ADVANCED_FACE('',(#1025,#487,#488,#489,#490,#491),#658,.T.);
#5999=ADVANCED_FACE('',(#1026),#5641,.F.);
#6000=ADVANCED_FACE('',(#1027,#492),#659,.F.);
#6001=ADVANCED_FACE('',(#1028,#493),#660,.T.);
#6002=ADVANCED_FACE('',(#1029),#5642,.T.);
#6003=ADVANCED_FACE('',(#1030),#5643,.F.);
#6004=ADVANCED_FACE('',(#1031,#494),#661,.F.);
#6005=ADVANCED_FACE('',(#1032,#495),#662,.T.);
#6006=ADVANCED_FACE('',(#1033),#5644,.T.);
#6007=ADVANCED_FACE('',(#1034),#5645,.T.);
#6008=ADVANCED_FACE('',(#1035),#663,.T.);
#6009=ADVANCED_FACE('',(#1036),#664,.F.);
#6010=CLOSED_SHELL('',(#5646,#5647,#5648,#5649,#5650,#5651,#5652,#5653,
#5654,#5655,#5656,#5657,#5658,#5659,#5660,#5661,#5662,#5663,#5664,#5665,
#5666,#5667));
#6011=CLOSED_SHELL('',(#5668,#5669,#5670,#5671,#5672,#5673,#5674,#5675,
#5676,#5677,#5678,#5679,#5680,#5681,#5682,#5683,#5684,#5685,#5686,#5687));
#6012=CLOSED_SHELL('',(#5688,#5689,#5690,#5691,#5692,#5693,#5694,#5695,
#5696,#5697,#5698,#5699,#5700,#5701,#5702,#5703,#5704,#5705,#5706,#5707));
#6013=CLOSED_SHELL('',(#5708,#5709,#5710,#5711,#5712,#5713,#5714,#5715,
#5716,#5717,#5718,#5719,#5720,#5721,#5722,#5723,#5724,#5725,#5726,#5727,
#5728,#5729));
#6014=CLOSED_SHELL('',(#5730,#5731,#5732,#5733,#5734,#5735,#5736,#5737,
#5738,#5739,#5740,#5741,#5742,#5743,#5744,#5745));
#6015=CLOSED_SHELL('',(#5746,#5747,#5748,#5749,#5750,#5751,#5752,#5753,
#5754,#5755,#5756));
#6016=CLOSED_SHELL('',(#5757,#5758,#5759,#5760,#5761,#5762,#5763,#5764,
#5765,#5766,#5767,#5768,#5769,#5770,#5771,#5772,#5773,#5774,#5775,#5776));
#6017=CLOSED_SHELL('',(#5777,#5778,#5779,#5780,#5781,#5782,#5783,#5784,
#5785,#5786,#5787,#5788,#5789));
#6018=CLOSED_SHELL('',(#5790,#5791,#5792,#5793,#5794,#5795,#5796,#5797,
#5798,#5799,#5800,#5801,#5802,#5803,#5804,#5805,#5806,#5807,#5808,#5809));
#6019=CLOSED_SHELL('',(#5810,#5811,#5812,#5813,#5814));
#6020=CLOSED_SHELL('',(#5815,#5816,#5817,#5818,#5819,#5820,#5821,#5822,
#5823,#5824,#5825,#5826,#5827));
#6021=CLOSED_SHELL('',(#5828,#5829,#5830,#5831,#5832));
#6022=CLOSED_SHELL('',(#5833,#5834,#5835,#5836,#5837,#5838,#5839,#5840,
#5841,#5842,#5843,#5844,#5845));
#6023=CLOSED_SHELL('',(#5846,#5847,#5848,#5849,#5850,#5851,#5852,#5853,
#5854,#5855,#5856,#5857,#5858));
#6024=CLOSED_SHELL('',(#5859,#5860,#5861,#5862,#5863));
#6025=CLOSED_SHELL('',(#5864,#5865,#5866,#5867,#5868,#5869,#5870,#5871,
#5872,#5873,#5874,#5875,#5876));
#6026=CLOSED_SHELL('',(#5877,#5878,#5879,#5880,#5881,#5882,#5883,#5884,
#5885,#5886,#5887,#5888,#5889,#5890,#5891,#5892,#5893,#5894,#5895,#5896,
#5897,#5898,#5899,#5900,#5901,#5902,#5903,#5904,#5905,#5906,#5907,#5908));
#6027=CLOSED_SHELL('',(#5909,#5910,#5911,#5912,#5913,#5914,#5915));
#6028=CLOSED_SHELL('',(#5916,#5917,#5918,#5919,#5920,#5921,#5922,#5923));
#6029=CLOSED_SHELL('',(#5924,#5925,#5926,#5927,#5928,#5929));
#6030=CLOSED_SHELL('',(#5930,#5931,#5932,#5933,#5934,#5935,#5936,#5937));
#6031=CLOSED_SHELL('',(#5938,#5939,#5940,#5941,#5942,#5943,#5944,#5945,
#5946,#5947,#5948,#5949,#5950,#5951,#5952,#5953));
#6032=CLOSED_SHELL('',(#5954,#5955,#5956,#5957,#5958,#5959,#5960,#5961));
#6033=CLOSED_SHELL('',(#5962,#5963,#5964,#5965,#5966,#5967,#5968,#5969));
#6034=CLOSED_SHELL('',(#5970,#5971,#5972));
#6035=CLOSED_SHELL('',(#5973,#5974,#5975));
#6036=CLOSED_SHELL('',(#5976,#5977,#5978,#5979));
#6037=CLOSED_SHELL('',(#5980,#5981,#5982));
#6038=CLOSED_SHELL('',(#5983,#5984,#5985));
#6039=CLOSED_SHELL('',(#5986,#5987,#5988,#5989,#5990,#5991,#5992,#5993,
#5994,#5995,#5996,#5997,#5998));
#6040=CLOSED_SHELL('',(#5999,#6000,#6001,#6002));
#6041=CLOSED_SHELL('',(#6003,#6004,#6005,#6006));
#6042=CLOSED_SHELL('',(#6007,#6008,#6009));
#6043=DERIVED_UNIT_ELEMENT(#6109,1.);
#6044=DERIVED_UNIT_ELEMENT(#11113,-3.);
#6045=DERIVED_UNIT_ELEMENT(#6109,1.);
#6046=DERIVED_UNIT_ELEMENT(#11113,-3.);
#6047=DERIVED_UNIT_ELEMENT(#6109,1.);
#6048=DERIVED_UNIT_ELEMENT(#11113,-3.);
#6049=DERIVED_UNIT_ELEMENT(#6109,1.);
#6050=DERIVED_UNIT_ELEMENT(#11113,-3.);
#6051=DERIVED_UNIT_ELEMENT(#6109,1.);
#6052=DERIVED_UNIT_ELEMENT(#11113,-3.);
#6053=DERIVED_UNIT_ELEMENT(#6109,1.);
#6054=DERIVED_UNIT_ELEMENT(#11113,-3.);
#6055=DERIVED_UNIT_ELEMENT(#6109,1.);
#6056=DERIVED_UNIT_ELEMENT(#11113,-3.);
#6057=DERIVED_UNIT_ELEMENT(#6109,1.);
#6058=DERIVED_UNIT_ELEMENT(#11113,-3.);
#6059=DERIVED_UNIT_ELEMENT(#6109,1.);
#6060=DERIVED_UNIT_ELEMENT(#11113,-3.);
#6061=DERIVED_UNIT_ELEMENT(#6109,1.);
#6062=DERIVED_UNIT_ELEMENT(#11113,-3.);
#6063=DERIVED_UNIT_ELEMENT(#6109,1.);
#6064=DERIVED_UNIT_ELEMENT(#11113,-3.);
#6065=DERIVED_UNIT_ELEMENT(#6109,1.);
#6066=DERIVED_UNIT_ELEMENT(#11113,-3.);
#6067=DERIVED_UNIT_ELEMENT(#6109,1.);
#6068=DERIVED_UNIT_ELEMENT(#11113,-3.);
#6069=DERIVED_UNIT_ELEMENT(#6109,1.);
#6070=DERIVED_UNIT_ELEMENT(#11113,-3.);
#6071=DERIVED_UNIT_ELEMENT(#6109,1.);
#6072=DERIVED_UNIT_ELEMENT(#11113,-3.);
#6073=DERIVED_UNIT_ELEMENT(#6109,1.);
#6074=DERIVED_UNIT_ELEMENT(#11113,-3.);
#6075=DERIVED_UNIT_ELEMENT(#6109,1.);
#6076=DERIVED_UNIT_ELEMENT(#11113,-3.);
#6077=DERIVED_UNIT_ELEMENT(#6109,1.);
#6078=DERIVED_UNIT_ELEMENT(#11113,-3.);
#6079=DERIVED_UNIT_ELEMENT(#6109,1.);
#6080=DERIVED_UNIT_ELEMENT(#11113,-3.);
#6081=DERIVED_UNIT_ELEMENT(#6109,1.);
#6082=DERIVED_UNIT_ELEMENT(#11113,-3.);
#6083=DERIVED_UNIT_ELEMENT(#6109,1.);
#6084=DERIVED_UNIT_ELEMENT(#11113,-3.);
#6085=DERIVED_UNIT_ELEMENT(#6109,1.);
#6086=DERIVED_UNIT_ELEMENT(#11113,-3.);
#6087=DERIVED_UNIT_ELEMENT(#6109,1.);
#6088=DERIVED_UNIT_ELEMENT(#11113,-3.);
#6089=DERIVED_UNIT_ELEMENT(#6109,1.);
#6090=DERIVED_UNIT_ELEMENT(#11113,-3.);
#6091=DERIVED_UNIT_ELEMENT(#6109,1.);
#6092=DERIVED_UNIT_ELEMENT(#11113,-3.);
#6093=DERIVED_UNIT_ELEMENT(#6109,1.);
#6094=DERIVED_UNIT_ELEMENT(#11113,-3.);
#6095=DERIVED_UNIT_ELEMENT(#6109,1.);
#6096=DERIVED_UNIT_ELEMENT(#11113,-3.);
#6097=DERIVED_UNIT_ELEMENT(#6109,1.);
#6098=DERIVED_UNIT_ELEMENT(#11113,-3.);
#6099=DERIVED_UNIT_ELEMENT(#6109,1.);
#6100=DERIVED_UNIT_ELEMENT(#11113,-3.);
#6101=DERIVED_UNIT_ELEMENT(#6109,1.);
#6102=DERIVED_UNIT_ELEMENT(#11113,-3.);
#6103=DERIVED_UNIT_ELEMENT(#6109,1.);
#6104=DERIVED_UNIT_ELEMENT(#11113,-3.);
#6105=DERIVED_UNIT_ELEMENT(#6109,1.);
#6106=DERIVED_UNIT_ELEMENT(#11113,-3.);
#6107=DERIVED_UNIT_ELEMENT(#6109,1.);
#6108=DERIVED_UNIT_ELEMENT(#11113,-3.);
#6109=(
MASS_UNIT()
NAMED_UNIT(*)
SI_UNIT(.KILO.,.GRAM.)
);
#6110=DERIVED_UNIT((#6043,#6044));
#6111=DERIVED_UNIT((#6045,#6046));
#6112=DERIVED_UNIT((#6047,#6048));
#6113=DERIVED_UNIT((#6049,#6050));
#6114=DERIVED_UNIT((#6051,#6052));
#6115=DERIVED_UNIT((#6053,#6054));
#6116=DERIVED_UNIT((#6055,#6056));
#6117=DERIVED_UNIT((#6057,#6058));
#6118=DERIVED_UNIT((#6059,#6060));
#6119=DERIVED_UNIT((#6061,#6062));
#6120=DERIVED_UNIT((#6063,#6064));
#6121=DERIVED_UNIT((#6065,#6066));
#6122=DERIVED_UNIT((#6067,#6068));
#6123=DERIVED_UNIT((#6069,#6070));
#6124=DERIVED_UNIT((#6071,#6072));
#6125=DERIVED_UNIT((#6073,#6074));
#6126=DERIVED_UNIT((#6075,#6076));
#6127=DERIVED_UNIT((#6077,#6078));
#6128=DERIVED_UNIT((#6079,#6080));
#6129=DERIVED_UNIT((#6081,#6082));
#6130=DERIVED_UNIT((#6083,#6084));
#6131=DERIVED_UNIT((#6085,#6086));
#6132=DERIVED_UNIT((#6087,#6088));
#6133=DERIVED_UNIT((#6089,#6090));
#6134=DERIVED_UNIT((#6091,#6092));
#6135=DERIVED_UNIT((#6093,#6094));
#6136=DERIVED_UNIT((#6095,#6096));
#6137=DERIVED_UNIT((#6097,#6098));
#6138=DERIVED_UNIT((#6099,#6100));
#6139=DERIVED_UNIT((#6101,#6102));
#6140=DERIVED_UNIT((#6103,#6104));
#6141=DERIVED_UNIT((#6105,#6106));
#6142=DERIVED_UNIT((#6107,#6108));
#6143=MEASURE_REPRESENTATION_ITEM('density measure',
POSITIVE_RATIO_MEASURE(7850.),#6110);
#6144=MEASURE_REPRESENTATION_ITEM('density measure',
POSITIVE_RATIO_MEASURE(7850.),#6111);
#6145=MEASURE_REPRESENTATION_ITEM('density measure',
POSITIVE_RATIO_MEASURE(7850.),#6112);
#6146=MEASURE_REPRESENTATION_ITEM('density measure',
POSITIVE_RATIO_MEASURE(7850.),#6113);
#6147=MEASURE_REPRESENTATION_ITEM('density measure',
POSITIVE_RATIO_MEASURE(7850.),#6114);
#6148=MEASURE_REPRESENTATION_ITEM('density measure',
POSITIVE_RATIO_MEASURE(7850.),#6115);
#6149=MEASURE_REPRESENTATION_ITEM('density measure',
POSITIVE_RATIO_MEASURE(7850.),#6116);
#6150=MEASURE_REPRESENTATION_ITEM('density measure',
POSITIVE_RATIO_MEASURE(7850.),#6117);
#6151=MEASURE_REPRESENTATION_ITEM('density measure',
POSITIVE_RATIO_MEASURE(7850.),#6118);
#6152=MEASURE_REPRESENTATION_ITEM('density measure',
POSITIVE_RATIO_MEASURE(7850.),#6119);
#6153=MEASURE_REPRESENTATION_ITEM('density measure',
POSITIVE_RATIO_MEASURE(7850.),#6120);
#6154=MEASURE_REPRESENTATION_ITEM('density measure',
POSITIVE_RATIO_MEASURE(7850.),#6121);
#6155=MEASURE_REPRESENTATION_ITEM('density measure',
POSITIVE_RATIO_MEASURE(7850.),#6122);
#6156=MEASURE_REPRESENTATION_ITEM('density measure',
POSITIVE_RATIO_MEASURE(7850.),#6123);
#6157=MEASURE_REPRESENTATION_ITEM('density measure',
POSITIVE_RATIO_MEASURE(7850.),#6124);
#6158=MEASURE_REPRESENTATION_ITEM('density measure',
POSITIVE_RATIO_MEASURE(7850.),#6125);
#6159=MEASURE_REPRESENTATION_ITEM('density measure',
POSITIVE_RATIO_MEASURE(7850.),#6126);
#6160=MEASURE_REPRESENTATION_ITEM('density measure',
POSITIVE_RATIO_MEASURE(7850.),#6127);
#6161=MEASURE_REPRESENTATION_ITEM('density measure',
POSITIVE_RATIO_MEASURE(7850.),#6128);
#6162=MEASURE_REPRESENTATION_ITEM('density measure',
POSITIVE_RATIO_MEASURE(7850.),#6129);
#6163=MEASURE_REPRESENTATION_ITEM('density measure',
POSITIVE_RATIO_MEASURE(7850.),#6130);
#6164=MEASURE_REPRESENTATION_ITEM('density measure',
POSITIVE_RATIO_MEASURE(7850.),#6131);
#6165=MEASURE_REPRESENTATION_ITEM('density measure',
POSITIVE_RATIO_MEASURE(7850.),#6132);
#6166=MEASURE_REPRESENTATION_ITEM('density measure',
POSITIVE_RATIO_MEASURE(7850.),#6133);
#6167=MEASURE_REPRESENTATION_ITEM('density measure',
POSITIVE_RATIO_MEASURE(7850.),#6134);
#6168=MEASURE_REPRESENTATION_ITEM('density measure',
POSITIVE_RATIO_MEASURE(7850.),#6135);
#6169=MEASURE_REPRESENTATION_ITEM('density measure',
POSITIVE_RATIO_MEASURE(7850.),#6136);
#6170=MEASURE_REPRESENTATION_ITEM('density measure',
POSITIVE_RATIO_MEASURE(7850.),#6137);
#6171=MEASURE_REPRESENTATION_ITEM('density measure',
POSITIVE_RATIO_MEASURE(7850.),#6138);
#6172=MEASURE_REPRESENTATION_ITEM('density measure',
POSITIVE_RATIO_MEASURE(7850.),#6139);
#6173=MEASURE_REPRESENTATION_ITEM('density measure',
POSITIVE_RATIO_MEASURE(7850.),#6140);
#6174=MEASURE_REPRESENTATION_ITEM('density measure',
POSITIVE_RATIO_MEASURE(7850.),#6141);
#6175=MEASURE_REPRESENTATION_ITEM('density measure',
POSITIVE_RATIO_MEASURE(7850.),#6142);
#6176=PROPERTY_DEFINITION_REPRESENTATION(#6341,#6242);
#6177=PROPERTY_DEFINITION_REPRESENTATION(#6342,#6243);
#6178=PROPERTY_DEFINITION_REPRESENTATION(#6343,#6244);
#6179=PROPERTY_DEFINITION_REPRESENTATION(#6344,#6245);
#6180=PROPERTY_DEFINITION_REPRESENTATION(#6345,#6246);
#6181=PROPERTY_DEFINITION_REPRESENTATION(#6346,#6247);
#6182=PROPERTY_DEFINITION_REPRESENTATION(#6347,#6248);
#6183=PROPERTY_DEFINITION_REPRESENTATION(#6348,#6249);
#6184=PROPERTY_DEFINITION_REPRESENTATION(#6349,#6250);
#6185=PROPERTY_DEFINITION_REPRESENTATION(#6350,#6251);
#6186=PROPERTY_DEFINITION_REPRESENTATION(#6351,#6252);
#6187=PROPERTY_DEFINITION_REPRESENTATION(#6352,#6253);
#6188=PROPERTY_DEFINITION_REPRESENTATION(#6353,#6254);
#6189=PROPERTY_DEFINITION_REPRESENTATION(#6354,#6255);
#6190=PROPERTY_DEFINITION_REPRESENTATION(#6355,#6256);
#6191=PROPERTY_DEFINITION_REPRESENTATION(#6356,#6257);
#6192=PROPERTY_DEFINITION_REPRESENTATION(#6357,#6258);
#6193=PROPERTY_DEFINITION_REPRESENTATION(#6358,#6259);
#6194=PROPERTY_DEFINITION_REPRESENTATION(#6359,#6260);
#6195=PROPERTY_DEFINITION_REPRESENTATION(#6360,#6261);
#6196=PROPERTY_DEFINITION_REPRESENTATION(#6361,#6262);
#6197=PROPERTY_DEFINITION_REPRESENTATION(#6362,#6263);
#6198=PROPERTY_DEFINITION_REPRESENTATION(#6363,#6264);
#6199=PROPERTY_DEFINITION_REPRESENTATION(#6364,#6265);
#6200=PROPERTY_DEFINITION_REPRESENTATION(#6365,#6266);
#6201=PROPERTY_DEFINITION_REPRESENTATION(#6366,#6267);
#6202=PROPERTY_DEFINITION_REPRESENTATION(#6367,#6268);
#6203=PROPERTY_DEFINITION_REPRESENTATION(#6368,#6269);
#6204=PROPERTY_DEFINITION_REPRESENTATION(#6369,#6270);
#6205=PROPERTY_DEFINITION_REPRESENTATION(#6370,#6271);
#6206=PROPERTY_DEFINITION_REPRESENTATION(#6371,#6272);
#6207=PROPERTY_DEFINITION_REPRESENTATION(#6372,#6273);
#6208=PROPERTY_DEFINITION_REPRESENTATION(#6373,#6274);
#6209=PROPERTY_DEFINITION_REPRESENTATION(#6374,#6275);
#6210=PROPERTY_DEFINITION_REPRESENTATION(#6375,#6276);
#6211=PROPERTY_DEFINITION_REPRESENTATION(#6376,#6277);
#6212=PROPERTY_DEFINITION_REPRESENTATION(#6377,#6278);
#6213=PROPERTY_DEFINITION_REPRESENTATION(#6378,#6279);
#6214=PROPERTY_DEFINITION_REPRESENTATION(#6379,#6280);
#6215=PROPERTY_DEFINITION_REPRESENTATION(#6380,#6281);
#6216=PROPERTY_DEFINITION_REPRESENTATION(#6381,#6282);
#6217=PROPERTY_DEFINITION_REPRESENTATION(#6382,#6283);
#6218=PROPERTY_DEFINITION_REPRESENTATION(#6383,#6284);
#6219=PROPERTY_DEFINITION_REPRESENTATION(#6384,#6285);
#6220=PROPERTY_DEFINITION_REPRESENTATION(#6385,#6286);
#6221=PROPERTY_DEFINITION_REPRESENTATION(#6386,#6287);
#6222=PROPERTY_DEFINITION_REPRESENTATION(#6387,#6288);
#6223=PROPERTY_DEFINITION_REPRESENTATION(#6388,#6289);
#6224=PROPERTY_DEFINITION_REPRESENTATION(#6389,#6290);
#6225=PROPERTY_DEFINITION_REPRESENTATION(#6390,#6291);
#6226=PROPERTY_DEFINITION_REPRESENTATION(#6391,#6292);
#6227=PROPERTY_DEFINITION_REPRESENTATION(#6392,#6293);
#6228=PROPERTY_DEFINITION_REPRESENTATION(#6393,#6294);
#6229=PROPERTY_DEFINITION_REPRESENTATION(#6394,#6295);
#6230=PROPERTY_DEFINITION_REPRESENTATION(#6395,#6296);
#6231=PROPERTY_DEFINITION_REPRESENTATION(#6396,#6297);
#6232=PROPERTY_DEFINITION_REPRESENTATION(#6397,#6298);
#6233=PROPERTY_DEFINITION_REPRESENTATION(#6398,#6299);
#6234=PROPERTY_DEFINITION_REPRESENTATION(#6399,#6300);
#6235=PROPERTY_DEFINITION_REPRESENTATION(#6400,#6301);
#6236=PROPERTY_DEFINITION_REPRESENTATION(#6401,#6302);
#6237=PROPERTY_DEFINITION_REPRESENTATION(#6402,#6303);
#6238=PROPERTY_DEFINITION_REPRESENTATION(#6403,#6304);
#6239=PROPERTY_DEFINITION_REPRESENTATION(#6404,#6305);
#6240=PROPERTY_DEFINITION_REPRESENTATION(#6405,#6306);
#6241=PROPERTY_DEFINITION_REPRESENTATION(#6406,#6307);
#6242=REPRESENTATION('material name',(#6308),#11075);
#6243=REPRESENTATION('density',(#6143),#11075);
#6244=REPRESENTATION('material name',(#6309),#11076);
#6245=REPRESENTATION('density',(#6144),#11076);
#6246=REPRESENTATION('material name',(#6310),#11077);
#6247=REPRESENTATION('density',(#6145),#11077);
#6248=REPRESENTATION('material name',(#6311),#11078);
#6249=REPRESENTATION('density',(#6146),#11078);
#6250=REPRESENTATION('material name',(#6312),#11079);
#6251=REPRESENTATION('density',(#6147),#11079);
#6252=REPRESENTATION('material name',(#6313),#11080);
#6253=REPRESENTATION('density',(#6148),#11080);
#6254=REPRESENTATION('material name',(#6314),#11081);
#6255=REPRESENTATION('density',(#6149),#11081);
#6256=REPRESENTATION('material name',(#6315),#11082);
#6257=REPRESENTATION('density',(#6150),#11082);
#6258=REPRESENTATION('material name',(#6316),#11083);
#6259=REPRESENTATION('density',(#6151),#11083);
#6260=REPRESENTATION('material name',(#6317),#11085);
#6261=REPRESENTATION('density',(#6152),#11085);
#6262=REPRESENTATION('material name',(#6318),#11086);
#6263=REPRESENTATION('density',(#6153),#11086);
#6264=REPRESENTATION('material name',(#6319),#11087);
#6265=REPRESENTATION('density',(#6154),#11087);
#6266=REPRESENTATION('material name',(#6320),#11088);
#6267=REPRESENTATION('density',(#6155),#11088);
#6268=REPRESENTATION('material name',(#6321),#11089);
#6269=REPRESENTATION('density',(#6156),#11089);
#6270=REPRESENTATION('material name',(#6322),#11090);
#6271=REPRESENTATION('density',(#6157),#11090);
#6272=REPRESENTATION('material name',(#6323),#11091);
#6273=REPRESENTATION('density',(#6158),#11091);
#6274=REPRESENTATION('material name',(#6324),#11092);
#6275=REPRESENTATION('density',(#6159),#11092);
#6276=REPRESENTATION('material name',(#6325),#11093);
#6277=REPRESENTATION('density',(#6160),#11093);
#6278=REPRESENTATION('material name',(#6326),#11095);
#6279=REPRESENTATION('density',(#6161),#11095);
#6280=REPRESENTATION('material name',(#6327),#11096);
#6281=REPRESENTATION('density',(#6162),#11096);
#6282=REPRESENTATION('material name',(#6328),#11097);
#6283=REPRESENTATION('density',(#6163),#11097);
#6284=REPRESENTATION('material name',(#6329),#11098);
#6285=REPRESENTATION('density',(#6164),#11098);
#6286=REPRESENTATION('material name',(#6330),#11099);
#6287=REPRESENTATION('density',(#6165),#11099);
#6288=REPRESENTATION('material name',(#6331),#11100);
#6289=REPRESENTATION('density',(#6166),#11100);
#6290=REPRESENTATION('material name',(#6332),#11102);
#6291=REPRESENTATION('density',(#6167),#11102);
#6292=REPRESENTATION('material name',(#6333),#11103);
#6293=REPRESENTATION('density',(#6168),#11103);
#6294=REPRESENTATION('material name',(#6334),#11104);
#6295=REPRESENTATION('density',(#6169),#11104);
#6296=REPRESENTATION('material name',(#6335),#11105);
#6297=REPRESENTATION('density',(#6170),#11105);
#6298=REPRESENTATION('material name',(#6336),#11106);
#6299=REPRESENTATION('density',(#6171),#11106);
#6300=REPRESENTATION('material name',(#6337),#11107);
#6301=REPRESENTATION('density',(#6172),#11107);
#6302=REPRESENTATION('material name',(#6338),#11109);
#6303=REPRESENTATION('density',(#6173),#11109);
#6304=REPRESENTATION('material name',(#6339),#11110);
#6305=REPRESENTATION('density',(#6174),#11110);
#6306=REPRESENTATION('material name',(#6340),#11111);
#6307=REPRESENTATION('density',(#6175),#11111);
#6308=DESCRIPTIVE_REPRESENTATION_ITEM('Steel','Steel');
#6309=DESCRIPTIVE_REPRESENTATION_ITEM('Steel','Steel');
#6310=DESCRIPTIVE_REPRESENTATION_ITEM('Steel','Steel');
#6311=DESCRIPTIVE_REPRESENTATION_ITEM('Steel','Steel');
#6312=DESCRIPTIVE_REPRESENTATION_ITEM('Steel','Steel');
#6313=DESCRIPTIVE_REPRESENTATION_ITEM('Steel','Steel');
#6314=DESCRIPTIVE_REPRESENTATION_ITEM('Steel','Steel');
#6315=DESCRIPTIVE_REPRESENTATION_ITEM('Steel','Steel');
#6316=DESCRIPTIVE_REPRESENTATION_ITEM('Steel','Steel');
#6317=DESCRIPTIVE_REPRESENTATION_ITEM('Steel','Steel');
#6318=DESCRIPTIVE_REPRESENTATION_ITEM('Steel','Steel');
#6319=DESCRIPTIVE_REPRESENTATION_ITEM('Steel','Steel');
#6320=DESCRIPTIVE_REPRESENTATION_ITEM('Steel','Steel');
#6321=DESCRIPTIVE_REPRESENTATION_ITEM('Steel','Steel');
#6322=DESCRIPTIVE_REPRESENTATION_ITEM('Steel','Steel');
#6323=DESCRIPTIVE_REPRESENTATION_ITEM('Steel','Steel');
#6324=DESCRIPTIVE_REPRESENTATION_ITEM('Steel','Steel');
#6325=DESCRIPTIVE_REPRESENTATION_ITEM('Steel','Steel');
#6326=DESCRIPTIVE_REPRESENTATION_ITEM('Steel','Steel');
#6327=DESCRIPTIVE_REPRESENTATION_ITEM('Steel','Steel');
#6328=DESCRIPTIVE_REPRESENTATION_ITEM('Steel','Steel');
#6329=DESCRIPTIVE_REPRESENTATION_ITEM('Steel','Steel');
#6330=DESCRIPTIVE_REPRESENTATION_ITEM('Steel','Steel');
#6331=DESCRIPTIVE_REPRESENTATION_ITEM('Steel','Steel');
#6332=DESCRIPTIVE_REPRESENTATION_ITEM('Steel','Steel');
#6333=DESCRIPTIVE_REPRESENTATION_ITEM('Steel','Steel');
#6334=DESCRIPTIVE_REPRESENTATION_ITEM('Steel','Steel');
#6335=DESCRIPTIVE_REPRESENTATION_ITEM('Steel','Steel');
#6336=DESCRIPTIVE_REPRESENTATION_ITEM('Steel','Steel');
#6337=DESCRIPTIVE_REPRESENTATION_ITEM('Steel','Steel');
#6338=DESCRIPTIVE_REPRESENTATION_ITEM('Steel','Steel');
#6339=DESCRIPTIVE_REPRESENTATION_ITEM('Steel','Steel');
#6340=DESCRIPTIVE_REPRESENTATION_ITEM('Steel','Steel');
#6341=PROPERTY_DEFINITION('material property','material name',#11269);
#6342=PROPERTY_DEFINITION('material property','density of part',#11269);
#6343=PROPERTY_DEFINITION('material property','material name',#11270);
#6344=PROPERTY_DEFINITION('material property','density of part',#11270);
#6345=PROPERTY_DEFINITION('material property','material name',#11271);
#6346=PROPERTY_DEFINITION('material property','density of part',#11271);
#6347=PROPERTY_DEFINITION('material property','material name',#11272);
#6348=PROPERTY_DEFINITION('material property','density of part',#11272);
#6349=PROPERTY_DEFINITION('material property','material name',#11273);
#6350=PROPERTY_DEFINITION('material property','density of part',#11273);
#6351=PROPERTY_DEFINITION('material property','material name',#11274);
#6352=PROPERTY_DEFINITION('material property','density of part',#11274);
#6353=PROPERTY_DEFINITION('material property','material name',#11275);
#6354=PROPERTY_DEFINITION('material property','density of part',#11275);
#6355=PROPERTY_DEFINITION('material property','material name',#11276);
#6356=PROPERTY_DEFINITION('material property','density of part',#11276);
#6357=PROPERTY_DEFINITION('material property','material name',#11277);
#6358=PROPERTY_DEFINITION('material property','density of part',#11277);
#6359=PROPERTY_DEFINITION('material property','material name',#11279);
#6360=PROPERTY_DEFINITION('material property','density of part',#11279);
#6361=PROPERTY_DEFINITION('material property','material name',#11280);
#6362=PROPERTY_DEFINITION('material property','density of part',#11280);
#6363=PROPERTY_DEFINITION('material property','material name',#11281);
#6364=PROPERTY_DEFINITION('material property','density of part',#11281);
#6365=PROPERTY_DEFINITION('material property','material name',#11282);
#6366=PROPERTY_DEFINITION('material property','density of part',#11282);
#6367=PROPERTY_DEFINITION('material property','material name',#11283);
#6368=PROPERTY_DEFINITION('material property','density of part',#11283);
#6369=PROPERTY_DEFINITION('material property','material name',#11284);
#6370=PROPERTY_DEFINITION('material property','density of part',#11284);
#6371=PROPERTY_DEFINITION('material property','material name',#11285);
#6372=PROPERTY_DEFINITION('material property','density of part',#11285);
#6373=PROPERTY_DEFINITION('material property','material name',#11286);
#6374=PROPERTY_DEFINITION('material property','density of part',#11286);
#6375=PROPERTY_DEFINITION('material property','material name',#11287);
#6376=PROPERTY_DEFINITION('material property','density of part',#11287);
#6377=PROPERTY_DEFINITION('material property','material name',#11289);
#6378=PROPERTY_DEFINITION('material property','density of part',#11289);
#6379=PROPERTY_DEFINITION('material property','material name',#11290);
#6380=PROPERTY_DEFINITION('material property','density of part',#11290);
#6381=PROPERTY_DEFINITION('material property','material name',#11291);
#6382=PROPERTY_DEFINITION('material property','density of part',#11291);
#6383=PROPERTY_DEFINITION('material property','material name',#11292);
#6384=PROPERTY_DEFINITION('material property','density of part',#11292);
#6385=PROPERTY_DEFINITION('material property','material name',#11293);
#6386=PROPERTY_DEFINITION('material property','density of part',#11293);
#6387=PROPERTY_DEFINITION('material property','material name',#11294);
#6388=PROPERTY_DEFINITION('material property','density of part',#11294);
#6389=PROPERTY_DEFINITION('material property','material name',#11296);
#6390=PROPERTY_DEFINITION('material property','density of part',#11296);
#6391=PROPERTY_DEFINITION('material property','material name',#11297);
#6392=PROPERTY_DEFINITION('material property','density of part',#11297);
#6393=PROPERTY_DEFINITION('material property','material name',#11298);
#6394=PROPERTY_DEFINITION('material property','density of part',#11298);
#6395=PROPERTY_DEFINITION('material property','material name',#11299);
#6396=PROPERTY_DEFINITION('material property','density of part',#11299);
#6397=PROPERTY_DEFINITION('material property','material name',#11300);
#6398=PROPERTY_DEFINITION('material property','density of part',#11300);
#6399=PROPERTY_DEFINITION('material property','material name',#11301);
#6400=PROPERTY_DEFINITION('material property','density of part',#11301);
#6401=PROPERTY_DEFINITION('material property','material name',#11303);
#6402=PROPERTY_DEFINITION('material property','density of part',#11303);
#6403=PROPERTY_DEFINITION('material property','material name',#11304);
#6404=PROPERTY_DEFINITION('material property','density of part',#11304);
#6405=PROPERTY_DEFINITION('material property','material name',#11305);
#6406=PROPERTY_DEFINITION('material property','density of part',#11305);
#6407=AXIS2_PLACEMENT_3D('',#9325,#7260,#7261);
#6408=AXIS2_PLACEMENT_3D('',#9326,#7262,#7263);
#6409=AXIS2_PLACEMENT_3D('',#9327,#7264,#7265);
#6410=AXIS2_PLACEMENT_3D('',#9329,#7266,#7267);
#6411=AXIS2_PLACEMENT_3D('',#9332,#7269,#7270);
#6412=AXIS2_PLACEMENT_3D('',#9333,#7271,#7272);
#6413=AXIS2_PLACEMENT_3D('',#9335,#7273,#7274);
#6414=AXIS2_PLACEMENT_3D('',#9339,#7276,#7277);
#6415=AXIS2_PLACEMENT_3D('',#9340,#7278,#7279);
#6416=AXIS2_PLACEMENT_3D('',#9341,#7280,#7281);
#6417=AXIS2_PLACEMENT_3D('',#9343,#7282,#7283);
#6418=AXIS2_PLACEMENT_3D('',#9345,#7285,#7286);
#6419=AXIS2_PLACEMENT_3D('',#9348,#7287,#7288);
#6420=AXIS2_PLACEMENT_3D('',#9350,#7290,#7291);
#6421=AXIS2_PLACEMENT_3D('',#9351,#7292,#7293);
#6422=AXIS2_PLACEMENT_3D('',#9353,#7294,#7295);
#6423=AXIS2_PLACEMENT_3D('',#9355,#7297,#7298);
#6424=AXIS2_PLACEMENT_3D('',#9358,#7300,#7301);
#6425=AXIS2_PLACEMENT_3D('',#9359,#7302,#7303);
#6426=AXIS2_PLACEMENT_3D('',#9361,#7304,#7305);
#6427=AXIS2_PLACEMENT_3D('',#9362,#7306,#7307);
#6428=AXIS2_PLACEMENT_3D('',#9364,#7308,#7309);
#6429=AXIS2_PLACEMENT_3D('',#9365,#7310,#7311);
#6430=AXIS2_PLACEMENT_3D('',#9367,#7312,#7313);
#6431=AXIS2_PLACEMENT_3D('',#9369,#7315,#7316);
#6432=AXIS2_PLACEMENT_3D('',#9372,#7318,#7319);
#6433=AXIS2_PLACEMENT_3D('',#9373,#7320,#7321);
#6434=AXIS2_PLACEMENT_3D('',#9375,#7322,#7323);
#6435=AXIS2_PLACEMENT_3D('',#9377,#7324,#7325);
#6436=AXIS2_PLACEMENT_3D('',#9379,#7326,#7327);
#6437=AXIS2_PLACEMENT_3D('',#9381,#7328,#7329);
#6438=AXIS2_PLACEMENT_3D('',#9383,#7330,#7331);
#6439=AXIS2_PLACEMENT_3D('',#9385,#7332,#7333);
#6440=AXIS2_PLACEMENT_3D('',#9387,#7334,#7335);
#6441=AXIS2_PLACEMENT_3D('',#9388,#7336,#7337);
#6442=AXIS2_PLACEMENT_3D('',#9390,#7338,#7339);
#6443=AXIS2_PLACEMENT_3D('',#9392,#7340,#7341);
#6444=AXIS2_PLACEMENT_3D('',#9394,#7342,#7343);
#6445=AXIS2_PLACEMENT_3D('',#9396,#7344,#7345);
#6446=AXIS2_PLACEMENT_3D('',#9398,#7346,#7347);
#6447=AXIS2_PLACEMENT_3D('',#9400,#7348,#7349);
#6448=AXIS2_PLACEMENT_3D('',#9402,#7350,#7351);
#6449=AXIS2_PLACEMENT_3D('',#9403,#7352,#7353);
#6450=AXIS2_PLACEMENT_3D('',#9405,#7354,#7355);
#6451=AXIS2_PLACEMENT_3D('',#9407,#7357,#7358);
#6452=AXIS2_PLACEMENT_3D('',#9409,#7360,#7361);
#6453=AXIS2_PLACEMENT_3D('',#9411,#7363,#7364);
#6454=AXIS2_PLACEMENT_3D('',#9413,#7366,#7367);
#6455=AXIS2_PLACEMENT_3D('',#9415,#7369,#7370);
#6456=AXIS2_PLACEMENT_3D('',#9417,#7372,#7373);
#6457=AXIS2_PLACEMENT_3D('',#9419,#7375,#7376);
#6458=AXIS2_PLACEMENT_3D('',#9422,#7378,#7379);
#6459=AXIS2_PLACEMENT_3D('',#9423,#7380,#7381);
#6460=AXIS2_PLACEMENT_3D('',#9424,#7382,#7383);
#6461=AXIS2_PLACEMENT_3D('',#9425,#7384,#7385);
#6462=AXIS2_PLACEMENT_3D('',#9426,#7386,#7387);
#6463=AXIS2_PLACEMENT_3D('',#9429,#7388,#7389);
#6464=AXIS2_PLACEMENT_3D('',#9431,#7390,#7391);
#6465=AXIS2_PLACEMENT_3D('',#9433,#7392,#7393);
#6466=AXIS2_PLACEMENT_3D('',#9434,#7394,#7395);
#6467=AXIS2_PLACEMENT_3D('',#9435,#7396,#7397);
#6468=AXIS2_PLACEMENT_3D('',#9436,#7398,#7399);
#6469=AXIS2_PLACEMENT_3D('',#9437,#7400,#7401);
#6470=AXIS2_PLACEMENT_3D('',#9438,#7402,#7403);
#6471=AXIS2_PLACEMENT_3D('',#9441,#7404,#7405);
#6472=AXIS2_PLACEMENT_3D('',#9442,#7406,#7407);
#6473=AXIS2_PLACEMENT_3D('',#9444,#7409,#7410);
#6474=AXIS2_PLACEMENT_3D('',#9446,#7411,#7412);
#6475=AXIS2_PLACEMENT_3D('',#9447,#7413,#7414);
#6476=AXIS2_PLACEMENT_3D('',#9449,#7415,#7416);
#6477=AXIS2_PLACEMENT_3D('',#9451,#7417,#7418);
#6478=AXIS2_PLACEMENT_3D('',#9452,#7419,#7420);
#6479=AXIS2_PLACEMENT_3D('',#9453,#7421,#7422);
#6480=AXIS2_PLACEMENT_3D('',#9457,#7424,#7425);
#6481=AXIS2_PLACEMENT_3D('',#9458,#7426,#7427);
#6482=AXIS2_PLACEMENT_3D('',#9459,#7428,#7429);
#6483=AXIS2_PLACEMENT_3D('',#9460,#7430,#7431);
#6484=AXIS2_PLACEMENT_3D('',#9461,#7432,#7433);
#6485=AXIS2_PLACEMENT_3D('',#9463,#7434,#7435);
#6486=AXIS2_PLACEMENT_3D('',#9464,#7436,#7437);
#6487=AXIS2_PLACEMENT_3D('',#9466,#7438,#7439);
#6488=AXIS2_PLACEMENT_3D('',#9468,#7440,#7441);
#6489=AXIS2_PLACEMENT_3D('',#9469,#7442,#7443);
#6490=AXIS2_PLACEMENT_3D('',#9470,#7444,#7445);
#6491=AXIS2_PLACEMENT_3D('',#9473,#7446,#7447);
#6492=AXIS2_PLACEMENT_3D('',#9474,#7448,#7449);
#6493=AXIS2_PLACEMENT_3D('',#9476,#7451,#7452);
#6494=AXIS2_PLACEMENT_3D('',#9479,#7454,#7455);
#6495=AXIS2_PLACEMENT_3D('',#9480,#7456,#7457);
#6496=AXIS2_PLACEMENT_3D('',#9483,#7458,#7459);
#6497=AXIS2_PLACEMENT_3D('',#9484,#7460,#7461);
#6498=AXIS2_PLACEMENT_3D('',#9485,#7462,#7463);
#6499=AXIS2_PLACEMENT_3D('',#9486,#7464,#7465);
#6500=AXIS2_PLACEMENT_3D('',#9489,#7466,#7467);
#6501=AXIS2_PLACEMENT_3D('',#9490,#7468,#7469);
#6502=AXIS2_PLACEMENT_3D('',#9491,#7470,#7471);
#6503=AXIS2_PLACEMENT_3D('',#9493,#7472,#7473);
#6504=AXIS2_PLACEMENT_3D('',#9495,#7475,#7476);
#6505=AXIS2_PLACEMENT_3D('',#9497,#7477,#7478);
#6506=AXIS2_PLACEMENT_3D('',#9499,#7479,#7480);
#6507=AXIS2_PLACEMENT_3D('',#9500,#7481,#7482);
#6508=AXIS2_PLACEMENT_3D('',#9501,#7483,#7484);
#6509=AXIS2_PLACEMENT_3D('',#9502,#7485,#7486);
#6510=AXIS2_PLACEMENT_3D('',#9503,#7487,#7488);
#6511=AXIS2_PLACEMENT_3D('',#9506,#7489,#7490);
#6512=AXIS2_PLACEMENT_3D('',#9507,#7491,#7492);
#6513=AXIS2_PLACEMENT_3D('',#9508,#7493,#7494);
#6514=AXIS2_PLACEMENT_3D('',#9512,#7496,#7497);
#6515=AXIS2_PLACEMENT_3D('',#9513,#7498,#7499);
#6516=AXIS2_PLACEMENT_3D('',#9514,#7500,#7501);
#6517=AXIS2_PLACEMENT_3D('',#9515,#7502,#7503);
#6518=AXIS2_PLACEMENT_3D('',#9516,#7504,#7505);
#6519=AXIS2_PLACEMENT_3D('',#9517,#7506,#7507);
#6520=AXIS2_PLACEMENT_3D('',#9518,#7508,#7509);
#6521=AXIS2_PLACEMENT_3D('',#9519,#7510,#7511);
#6522=AXIS2_PLACEMENT_3D('',#9522,#7512,#7513);
#6523=AXIS2_PLACEMENT_3D('',#9524,#7514,#7515);
#6524=AXIS2_PLACEMENT_3D('',#9526,#7516,#7517);
#6525=AXIS2_PLACEMENT_3D('',#9527,#7518,#7519);
#6526=AXIS2_PLACEMENT_3D('',#9528,#7520,#7521);
#6527=AXIS2_PLACEMENT_3D('',#9529,#7522,#7523);
#6528=AXIS2_PLACEMENT_3D('',#9530,#7524,#7525);
#6529=AXIS2_PLACEMENT_3D('',#9531,#7526,#7527);
#6530=AXIS2_PLACEMENT_3D('',#9534,#7528,#7529);
#6531=AXIS2_PLACEMENT_3D('',#9535,#7530,#7531);
#6532=AXIS2_PLACEMENT_3D('',#9537,#7533,#7534);
#6533=AXIS2_PLACEMENT_3D('',#9539,#7535,#7536);
#6534=AXIS2_PLACEMENT_3D('',#9540,#7537,#7538);
#6535=AXIS2_PLACEMENT_3D('',#9542,#7539,#7540);
#6536=AXIS2_PLACEMENT_3D('',#9544,#7541,#7542);
#6537=AXIS2_PLACEMENT_3D('',#9545,#7543,#7544);
#6538=AXIS2_PLACEMENT_3D('',#9546,#7545,#7546);
#6539=AXIS2_PLACEMENT_3D('',#9550,#7548,#7549);
#6540=AXIS2_PLACEMENT_3D('',#9551,#7550,#7551);
#6541=AXIS2_PLACEMENT_3D('',#9552,#7552,#7553);
#6542=AXIS2_PLACEMENT_3D('',#9553,#7554,#7555);
#6543=AXIS2_PLACEMENT_3D('',#9554,#7556,#7557);
#6544=AXIS2_PLACEMENT_3D('',#9556,#7558,#7559);
#6545=AXIS2_PLACEMENT_3D('',#9557,#7560,#7561);
#6546=AXIS2_PLACEMENT_3D('',#9559,#7562,#7563);
#6547=AXIS2_PLACEMENT_3D('',#9561,#7564,#7565);
#6548=AXIS2_PLACEMENT_3D('',#9562,#7566,#7567);
#6549=AXIS2_PLACEMENT_3D('',#9563,#7568,#7569);
#6550=AXIS2_PLACEMENT_3D('',#9566,#7570,#7571);
#6551=AXIS2_PLACEMENT_3D('',#9567,#7572,#7573);
#6552=AXIS2_PLACEMENT_3D('',#9569,#7575,#7576);
#6553=AXIS2_PLACEMENT_3D('',#9572,#7578,#7579);
#6554=AXIS2_PLACEMENT_3D('',#9573,#7580,#7581);
#6555=AXIS2_PLACEMENT_3D('',#9576,#7582,#7583);
#6556=AXIS2_PLACEMENT_3D('',#9577,#7584,#7585);
#6557=AXIS2_PLACEMENT_3D('',#9578,#7586,#7587);
#6558=AXIS2_PLACEMENT_3D('',#9579,#7588,#7589);
#6559=AXIS2_PLACEMENT_3D('',#9582,#7590,#7591);
#6560=AXIS2_PLACEMENT_3D('',#9583,#7592,#7593);
#6561=AXIS2_PLACEMENT_3D('',#9584,#7594,#7595);
#6562=AXIS2_PLACEMENT_3D('',#9586,#7596,#7597);
#6563=AXIS2_PLACEMENT_3D('',#9588,#7599,#7600);
#6564=AXIS2_PLACEMENT_3D('',#9590,#7601,#7602);
#6565=AXIS2_PLACEMENT_3D('',#9592,#7603,#7604);
#6566=AXIS2_PLACEMENT_3D('',#9593,#7605,#7606);
#6567=AXIS2_PLACEMENT_3D('',#9594,#7607,#7608);
#6568=AXIS2_PLACEMENT_3D('',#9595,#7609,#7610);
#6569=AXIS2_PLACEMENT_3D('',#9596,#7611,#7612);
#6570=AXIS2_PLACEMENT_3D('',#9599,#7613,#7614);
#6571=AXIS2_PLACEMENT_3D('',#9600,#7615,#7616);
#6572=AXIS2_PLACEMENT_3D('',#9601,#7617,#7618);
#6573=AXIS2_PLACEMENT_3D('',#9605,#7620,#7621);
#6574=AXIS2_PLACEMENT_3D('',#9606,#7622,#7623);
#6575=AXIS2_PLACEMENT_3D('',#9607,#7624,#7625);
#6576=AXIS2_PLACEMENT_3D('',#9608,#7626,#7627);
#6577=AXIS2_PLACEMENT_3D('',#9609,#7628,#7629);
#6578=AXIS2_PLACEMENT_3D('',#9610,#7630,#7631);
#6579=AXIS2_PLACEMENT_3D('',#9611,#7632,#7633);
#6580=AXIS2_PLACEMENT_3D('',#9612,#7634,#7635);
#6581=AXIS2_PLACEMENT_3D('',#9614,#7636,#7637);
#6582=AXIS2_PLACEMENT_3D('',#9618,#7639,#7640);
#6583=AXIS2_PLACEMENT_3D('',#9619,#7641,#7642);
#6584=AXIS2_PLACEMENT_3D('',#9620,#7643,#7644);
#6585=AXIS2_PLACEMENT_3D('',#9622,#7645,#7646);
#6586=AXIS2_PLACEMENT_3D('',#9624,#7648,#7649);
#6587=AXIS2_PLACEMENT_3D('',#9627,#7650,#7651);
#6588=AXIS2_PLACEMENT_3D('',#9629,#7653,#7654);
#6589=AXIS2_PLACEMENT_3D('',#9630,#7655,#7656);
#6590=AXIS2_PLACEMENT_3D('',#9632,#7657,#7658);
#6591=AXIS2_PLACEMENT_3D('',#9634,#7660,#7661);
#6592=AXIS2_PLACEMENT_3D('',#9637,#7663,#7664);
#6593=AXIS2_PLACEMENT_3D('',#9638,#7665,#7666);
#6594=AXIS2_PLACEMENT_3D('',#9640,#7667,#7668);
#6595=AXIS2_PLACEMENT_3D('',#9641,#7669,#7670);
#6596=AXIS2_PLACEMENT_3D('',#9643,#7671,#7672);
#6597=AXIS2_PLACEMENT_3D('',#9644,#7673,#7674);
#6598=AXIS2_PLACEMENT_3D('',#9646,#7675,#7676);
#6599=AXIS2_PLACEMENT_3D('',#9648,#7678,#7679);
#6600=AXIS2_PLACEMENT_3D('',#9651,#7681,#7682);
#6601=AXIS2_PLACEMENT_3D('',#9652,#7683,#7684);
#6602=AXIS2_PLACEMENT_3D('',#9654,#7685,#7686);
#6603=AXIS2_PLACEMENT_3D('',#9656,#7687,#7688);
#6604=AXIS2_PLACEMENT_3D('',#9658,#7689,#7690);
#6605=AXIS2_PLACEMENT_3D('',#9660,#7691,#7692);
#6606=AXIS2_PLACEMENT_3D('',#9662,#7693,#7694);
#6607=AXIS2_PLACEMENT_3D('',#9664,#7695,#7696);
#6608=AXIS2_PLACEMENT_3D('',#9666,#7697,#7698);
#6609=AXIS2_PLACEMENT_3D('',#9667,#7699,#7700);
#6610=AXIS2_PLACEMENT_3D('',#9669,#7701,#7702);
#6611=AXIS2_PLACEMENT_3D('',#9671,#7703,#7704);
#6612=AXIS2_PLACEMENT_3D('',#9673,#7705,#7706);
#6613=AXIS2_PLACEMENT_3D('',#9675,#7707,#7708);
#6614=AXIS2_PLACEMENT_3D('',#9677,#7709,#7710);
#6615=AXIS2_PLACEMENT_3D('',#9679,#7711,#7712);
#6616=AXIS2_PLACEMENT_3D('',#9681,#7713,#7714);
#6617=AXIS2_PLACEMENT_3D('',#9682,#7715,#7716);
#6618=AXIS2_PLACEMENT_3D('',#9684,#7717,#7718);
#6619=AXIS2_PLACEMENT_3D('',#9686,#7720,#7721);
#6620=AXIS2_PLACEMENT_3D('',#9688,#7723,#7724);
#6621=AXIS2_PLACEMENT_3D('',#9690,#7726,#7727);
#6622=AXIS2_PLACEMENT_3D('',#9692,#7729,#7730);
#6623=AXIS2_PLACEMENT_3D('',#9694,#7732,#7733);
#6624=AXIS2_PLACEMENT_3D('',#9696,#7735,#7736);
#6625=AXIS2_PLACEMENT_3D('',#9698,#7738,#7739);
#6626=AXIS2_PLACEMENT_3D('',#9701,#7741,#7742);
#6627=AXIS2_PLACEMENT_3D('',#9702,#7743,#7744);
#6628=AXIS2_PLACEMENT_3D('',#9704,#7745,#7746);
#6629=AXIS2_PLACEMENT_3D('',#9705,#7747,#7748);
#6630=AXIS2_PLACEMENT_3D('',#9707,#7749,#7750);
#6631=AXIS2_PLACEMENT_3D('',#9708,#7751,#7752);
#6632=AXIS2_PLACEMENT_3D('',#9710,#7754,#7755);
#6633=AXIS2_PLACEMENT_3D('',#9711,#7756,#7757);
#6634=AXIS2_PLACEMENT_3D('',#9714,#7758,#7759);
#6635=AXIS2_PLACEMENT_3D('',#9718,#7761,#7762);
#6636=AXIS2_PLACEMENT_3D('',#9720,#7764,#7765);
#6637=AXIS2_PLACEMENT_3D('',#9726,#7769,#7770);
#6638=AXIS2_PLACEMENT_3D('',#9730,#7772,#7773);
#6639=AXIS2_PLACEMENT_3D('',#9732,#7775,#7776);
#6640=AXIS2_PLACEMENT_3D('',#9735,#7777,#7778);
#6641=AXIS2_PLACEMENT_3D('',#9738,#7781,#7782);
#6642=AXIS2_PLACEMENT_3D('',#9742,#7785,#7786);
#6643=AXIS2_PLACEMENT_3D('',#9746,#7788,#7789);
#6644=AXIS2_PLACEMENT_3D('',#9747,#7790,#7791);
#6645=AXIS2_PLACEMENT_3D('',#9748,#7792,#7793);
#6646=AXIS2_PLACEMENT_3D('',#9752,#7796,#7797);
#6647=AXIS2_PLACEMENT_3D('',#9755,#7800,#7801);
#6648=AXIS2_PLACEMENT_3D('',#9758,#7804,#7805);
#6649=AXIS2_PLACEMENT_3D('',#9762,#7808,#7809);
#6650=AXIS2_PLACEMENT_3D('',#9764,#7811,#7812);
#6651=AXIS2_PLACEMENT_3D('',#9766,#7813,#7814);
#6652=AXIS2_PLACEMENT_3D('',#9768,#7816,#7817);
#6653=AXIS2_PLACEMENT_3D('',#9769,#7818,#7819);
#6654=AXIS2_PLACEMENT_3D('',#9770,#7820,#7821);
#6655=AXIS2_PLACEMENT_3D('',#9772,#7823,#7824);
#6656=AXIS2_PLACEMENT_3D('',#9774,#7826,#7827);
#6657=AXIS2_PLACEMENT_3D('',#9775,#7828,#7829);
#6658=AXIS2_PLACEMENT_3D('',#9776,#7830,#7831);
#6659=AXIS2_PLACEMENT_3D('',#9778,#7832,#7833);
#6660=AXIS2_PLACEMENT_3D('',#9781,#7835,#7836);
#6661=AXIS2_PLACEMENT_3D('',#9782,#7837,#7838);
#6662=AXIS2_PLACEMENT_3D('',#9792,#7843,#7844);
#6663=AXIS2_PLACEMENT_3D('',#9794,#7845,#7846);
#6664=AXIS2_PLACEMENT_3D('',#9796,#7847,#7848);
#6665=AXIS2_PLACEMENT_3D('',#9798,#7849,#7850);
#6666=AXIS2_PLACEMENT_3D('',#9799,#7851,#7852);
#6667=AXIS2_PLACEMENT_3D('',#9809,#7857,#7858);
#6668=AXIS2_PLACEMENT_3D('',#9811,#7859,#7860);
#6669=AXIS2_PLACEMENT_3D('',#9813,#7861,#7862);
#6670=AXIS2_PLACEMENT_3D('',#9815,#7863,#7864);
#6671=AXIS2_PLACEMENT_3D('',#9816,#7865,#7866);
#6672=AXIS2_PLACEMENT_3D('',#9818,#7868,#7869);
#6673=AXIS2_PLACEMENT_3D('',#9820,#7871,#7872);
#6674=AXIS2_PLACEMENT_3D('',#9822,#7874,#7875);
#6675=AXIS2_PLACEMENT_3D('',#9824,#7877,#7878);
#6676=AXIS2_PLACEMENT_3D('',#9827,#7881,#7882);
#6677=AXIS2_PLACEMENT_3D('',#9829,#7884,#7885);
#6678=AXIS2_PLACEMENT_3D('',#9831,#7887,#7888);
#6679=AXIS2_PLACEMENT_3D('',#9832,#7889,#7890);
#6680=AXIS2_PLACEMENT_3D('',#9833,#7891,#7892);
#6681=AXIS2_PLACEMENT_3D('',#9836,#7893,#7894);
#6682=AXIS2_PLACEMENT_3D('',#9838,#7895,#7896);
#6683=AXIS2_PLACEMENT_3D('',#9840,#7897,#7898);
#6684=AXIS2_PLACEMENT_3D('',#9841,#7899,#7900);
#6685=AXIS2_PLACEMENT_3D('',#9842,#7901,#7902);
#6686=AXIS2_PLACEMENT_3D('',#9843,#7903,#7904);
#6687=AXIS2_PLACEMENT_3D('',#9844,#7905,#7906);
#6688=AXIS2_PLACEMENT_3D('',#9845,#7907,#7908);
#6689=AXIS2_PLACEMENT_3D('',#9848,#7909,#7910);
#6690=AXIS2_PLACEMENT_3D('',#9849,#7911,#7912);
#6691=AXIS2_PLACEMENT_3D('',#9851,#7914,#7915);
#6692=AXIS2_PLACEMENT_3D('',#9853,#7916,#7917);
#6693=AXIS2_PLACEMENT_3D('',#9854,#7918,#7919);
#6694=AXIS2_PLACEMENT_3D('',#9856,#7920,#7921);
#6695=AXIS2_PLACEMENT_3D('',#9858,#7922,#7923);
#6696=AXIS2_PLACEMENT_3D('',#9859,#7924,#7925);
#6697=AXIS2_PLACEMENT_3D('',#9860,#7926,#7927);
#6698=AXIS2_PLACEMENT_3D('',#9864,#7929,#7930);
#6699=AXIS2_PLACEMENT_3D('',#9865,#7931,#7932);
#6700=AXIS2_PLACEMENT_3D('',#9866,#7933,#7934);
#6701=AXIS2_PLACEMENT_3D('',#9867,#7935,#7936);
#6702=AXIS2_PLACEMENT_3D('',#9868,#7937,#7938);
#6703=AXIS2_PLACEMENT_3D('',#9870,#7939,#7940);
#6704=AXIS2_PLACEMENT_3D('',#9871,#7941,#7942);
#6705=AXIS2_PLACEMENT_3D('',#9873,#7943,#7944);
#6706=AXIS2_PLACEMENT_3D('',#9875,#7945,#7946);
#6707=AXIS2_PLACEMENT_3D('',#9876,#7947,#7948);
#6708=AXIS2_PLACEMENT_3D('',#9877,#7949,#7950);
#6709=AXIS2_PLACEMENT_3D('',#9880,#7951,#7952);
#6710=AXIS2_PLACEMENT_3D('',#9881,#7953,#7954);
#6711=AXIS2_PLACEMENT_3D('',#9883,#7956,#7957);
#6712=AXIS2_PLACEMENT_3D('',#9886,#7959,#7960);
#6713=AXIS2_PLACEMENT_3D('',#9887,#7961,#7962);
#6714=AXIS2_PLACEMENT_3D('',#9890,#7963,#7964);
#6715=AXIS2_PLACEMENT_3D('',#9891,#7965,#7966);
#6716=AXIS2_PLACEMENT_3D('',#9892,#7967,#7968);
#6717=AXIS2_PLACEMENT_3D('',#9893,#7969,#7970);
#6718=AXIS2_PLACEMENT_3D('',#9896,#7971,#7972);
#6719=AXIS2_PLACEMENT_3D('',#9897,#7973,#7974);
#6720=AXIS2_PLACEMENT_3D('',#9898,#7975,#7976);
#6721=AXIS2_PLACEMENT_3D('',#9900,#7977,#7978);
#6722=AXIS2_PLACEMENT_3D('',#9902,#7980,#7981);
#6723=AXIS2_PLACEMENT_3D('',#9904,#7982,#7983);
#6724=AXIS2_PLACEMENT_3D('',#9906,#7984,#7985);
#6725=AXIS2_PLACEMENT_3D('',#9907,#7986,#7987);
#6726=AXIS2_PLACEMENT_3D('',#9908,#7988,#7989);
#6727=AXIS2_PLACEMENT_3D('',#9909,#7990,#7991);
#6728=AXIS2_PLACEMENT_3D('',#9910,#7992,#7993);
#6729=AXIS2_PLACEMENT_3D('',#9913,#7994,#7995);
#6730=AXIS2_PLACEMENT_3D('',#9914,#7996,#7997);
#6731=AXIS2_PLACEMENT_3D('',#9915,#7998,#7999);
#6732=AXIS2_PLACEMENT_3D('',#9919,#8001,#8002);
#6733=AXIS2_PLACEMENT_3D('',#9920,#8003,#8004);
#6734=AXIS2_PLACEMENT_3D('',#9921,#8005,#8006);
#6735=AXIS2_PLACEMENT_3D('',#9922,#8007,#8008);
#6736=AXIS2_PLACEMENT_3D('',#9923,#8009,#8010);
#6737=AXIS2_PLACEMENT_3D('',#9924,#8011,#8012);
#6738=AXIS2_PLACEMENT_3D('',#9925,#8013,#8014);
#6739=AXIS2_PLACEMENT_3D('',#9926,#8015,#8016);
#6740=AXIS2_PLACEMENT_3D('',#9928,#8017,#8018);
#6741=AXIS2_PLACEMENT_3D('',#9931,#8020,#8021);
#6742=AXIS2_PLACEMENT_3D('',#9932,#8022,#8023);
#6743=AXIS2_PLACEMENT_3D('',#9934,#8024,#8025);
#6744=AXIS2_PLACEMENT_3D('',#9935,#8026,#8027);
#6745=AXIS2_PLACEMENT_3D('',#9938,#8028,#8029);
#6746=AXIS2_PLACEMENT_3D('',#9943,#8032,#8033);
#6747=AXIS2_PLACEMENT_3D('',#9945,#8034,#8035);
#6748=AXIS2_PLACEMENT_3D('',#9947,#8036,#8037);
#6749=AXIS2_PLACEMENT_3D('',#9949,#8038,#8039);
#6750=AXIS2_PLACEMENT_3D('',#9951,#8040,#8041);
#6751=AXIS2_PLACEMENT_3D('',#9952,#8042,#8043);
#6752=AXIS2_PLACEMENT_3D('',#9954,#8044,#8045);
#6753=AXIS2_PLACEMENT_3D('',#9956,#8047,#8048);
#6754=AXIS2_PLACEMENT_3D('',#9958,#8049,#8050);
#6755=AXIS2_PLACEMENT_3D('',#9960,#8052,#8053);
#6756=AXIS2_PLACEMENT_3D('',#9962,#8054,#8055);
#6757=AXIS2_PLACEMENT_3D('',#9964,#8057,#8058);
#6758=AXIS2_PLACEMENT_3D('',#9966,#8059,#8060);
#6759=AXIS2_PLACEMENT_3D('',#9968,#8062,#8063);
#6760=AXIS2_PLACEMENT_3D('',#9970,#8064,#8065);
#6761=AXIS2_PLACEMENT_3D('',#9972,#8067,#8068);
#6762=AXIS2_PLACEMENT_3D('',#9978,#8072,#8073);
#6763=AXIS2_PLACEMENT_3D('',#9982,#8076,#8077);
#6764=AXIS2_PLACEMENT_3D('',#9985,#8079,#8080);
#6765=AXIS2_PLACEMENT_3D('',#9986,#8081,#8082);
#6766=AXIS2_PLACEMENT_3D('',#9987,#8083,#8084);
#6767=AXIS2_PLACEMENT_3D('',#9988,#8085,#8086);
#6768=AXIS2_PLACEMENT_3D('',#9989,#8087,#8088);
#6769=AXIS2_PLACEMENT_3D('',#9990,#8089,#8090);
#6770=AXIS2_PLACEMENT_3D('',#9993,#8091,#8092);
#6771=AXIS2_PLACEMENT_3D('',#9995,#8093,#8094);
#6772=AXIS2_PLACEMENT_3D('',#9997,#8095,#8096);
#6773=AXIS2_PLACEMENT_3D('',#9998,#8097,#8098);
#6774=AXIS2_PLACEMENT_3D('',#9999,#8099,#8100);
#6775=AXIS2_PLACEMENT_3D('',#10000,#8101,#8102);
#6776=AXIS2_PLACEMENT_3D('',#10001,#8103,#8104);
#6777=AXIS2_PLACEMENT_3D('',#10002,#8105,#8106);
#6778=AXIS2_PLACEMENT_3D('',#10005,#8107,#8108);
#6779=AXIS2_PLACEMENT_3D('',#10006,#8109,#8110);
#6780=AXIS2_PLACEMENT_3D('',#10008,#8112,#8113);
#6781=AXIS2_PLACEMENT_3D('',#10010,#8114,#8115);
#6782=AXIS2_PLACEMENT_3D('',#10011,#8116,#8117);
#6783=AXIS2_PLACEMENT_3D('',#10013,#8118,#8119);
#6784=AXIS2_PLACEMENT_3D('',#10015,#8120,#8121);
#6785=AXIS2_PLACEMENT_3D('',#10016,#8122,#8123);
#6786=AXIS2_PLACEMENT_3D('',#10017,#8124,#8125);
#6787=AXIS2_PLACEMENT_3D('',#10021,#8127,#8128);
#6788=AXIS2_PLACEMENT_3D('',#10022,#8129,#8130);
#6789=AXIS2_PLACEMENT_3D('',#10023,#8131,#8132);
#6790=AXIS2_PLACEMENT_3D('',#10024,#8133,#8134);
#6791=AXIS2_PLACEMENT_3D('',#10025,#8135,#8136);
#6792=AXIS2_PLACEMENT_3D('',#10027,#8137,#8138);
#6793=AXIS2_PLACEMENT_3D('',#10028,#8139,#8140);
#6794=AXIS2_PLACEMENT_3D('',#10030,#8141,#8142);
#6795=AXIS2_PLACEMENT_3D('',#10032,#8143,#8144);
#6796=AXIS2_PLACEMENT_3D('',#10033,#8145,#8146);
#6797=AXIS2_PLACEMENT_3D('',#10034,#8147,#8148);
#6798=AXIS2_PLACEMENT_3D('',#10037,#8149,#8150);
#6799=AXIS2_PLACEMENT_3D('',#10038,#8151,#8152);
#6800=AXIS2_PLACEMENT_3D('',#10040,#8154,#8155);
#6801=AXIS2_PLACEMENT_3D('',#10043,#8157,#8158);
#6802=AXIS2_PLACEMENT_3D('',#10044,#8159,#8160);
#6803=AXIS2_PLACEMENT_3D('',#10047,#8161,#8162);
#6804=AXIS2_PLACEMENT_3D('',#10048,#8163,#8164);
#6805=AXIS2_PLACEMENT_3D('',#10049,#8165,#8166);
#6806=AXIS2_PLACEMENT_3D('',#10050,#8167,#8168);
#6807=AXIS2_PLACEMENT_3D('',#10053,#8169,#8170);
#6808=AXIS2_PLACEMENT_3D('',#10054,#8171,#8172);
#6809=AXIS2_PLACEMENT_3D('',#10055,#8173,#8174);
#6810=AXIS2_PLACEMENT_3D('',#10057,#8175,#8176);
#6811=AXIS2_PLACEMENT_3D('',#10059,#8178,#8179);
#6812=AXIS2_PLACEMENT_3D('',#10061,#8180,#8181);
#6813=AXIS2_PLACEMENT_3D('',#10063,#8182,#8183);
#6814=AXIS2_PLACEMENT_3D('',#10064,#8184,#8185);
#6815=AXIS2_PLACEMENT_3D('',#10065,#8186,#8187);
#6816=AXIS2_PLACEMENT_3D('',#10066,#8188,#8189);
#6817=AXIS2_PLACEMENT_3D('',#10067,#8190,#8191);
#6818=AXIS2_PLACEMENT_3D('',#10070,#8192,#8193);
#6819=AXIS2_PLACEMENT_3D('',#10071,#8194,#8195);
#6820=AXIS2_PLACEMENT_3D('',#10072,#8196,#8197);
#6821=AXIS2_PLACEMENT_3D('',#10076,#8199,#8200);
#6822=AXIS2_PLACEMENT_3D('',#10077,#8201,#8202);
#6823=AXIS2_PLACEMENT_3D('',#10078,#8203,#8204);
#6824=AXIS2_PLACEMENT_3D('',#10079,#8205,#8206);
#6825=AXIS2_PLACEMENT_3D('',#10080,#8207,#8208);
#6826=AXIS2_PLACEMENT_3D('',#10081,#8209,#8210);
#6827=AXIS2_PLACEMENT_3D('',#10082,#8211,#8212);
#6828=AXIS2_PLACEMENT_3D('',#10083,#8213,#8214);
#6829=AXIS2_PLACEMENT_3D('',#10084,#8215,#8216);
#6830=AXIS2_PLACEMENT_3D('',#10086,#8217,#8218);
#6831=AXIS2_PLACEMENT_3D('',#10089,#8220,#8221);
#6832=AXIS2_PLACEMENT_3D('',#10090,#8222,#8223);
#6833=AXIS2_PLACEMENT_3D('',#10091,#8224,#8225);
#6834=AXIS2_PLACEMENT_3D('',#10093,#8226,#8227);
#6835=AXIS2_PLACEMENT_3D('',#10094,#8228,#8229);
#6836=AXIS2_PLACEMENT_3D('',#10096,#8230,#8231);
#6837=AXIS2_PLACEMENT_3D('',#10098,#8233,#8234);
#6838=AXIS2_PLACEMENT_3D('',#10099,#8235,#8236);
#6839=AXIS2_PLACEMENT_3D('',#10100,#8237,#8238);
#6840=AXIS2_PLACEMENT_3D('',#10103,#8239,#8240);
#6841=AXIS2_PLACEMENT_3D('',#10105,#8241,#8242);
#6842=AXIS2_PLACEMENT_3D('',#10107,#8243,#8244);
#6843=AXIS2_PLACEMENT_3D('',#10109,#8245,#8246);
#6844=AXIS2_PLACEMENT_3D('',#10112,#8248,#8249);
#6845=AXIS2_PLACEMENT_3D('',#10114,#8250,#8251);
#6846=AXIS2_PLACEMENT_3D('',#10116,#8252,#8253);
#6847=AXIS2_PLACEMENT_3D('',#10117,#8254,#8255);
#6848=AXIS2_PLACEMENT_3D('',#10118,#8256,#8257);
#6849=AXIS2_PLACEMENT_3D('',#10119,#8258,#8259);
#6850=AXIS2_PLACEMENT_3D('',#10121,#8261,#8262);
#6851=AXIS2_PLACEMENT_3D('',#10125,#8265,#8266);
#6852=AXIS2_PLACEMENT_3D('',#10129,#8269,#8270);
#6853=AXIS2_PLACEMENT_3D('',#10131,#8272,#8273);
#6854=AXIS2_PLACEMENT_3D('',#10135,#8276,#8277);
#6855=AXIS2_PLACEMENT_3D('',#10139,#8280,#8281);
#6856=AXIS2_PLACEMENT_3D('',#10145,#8285,#8286);
#6857=AXIS2_PLACEMENT_3D('',#10149,#8289,#8290);
#6858=AXIS2_PLACEMENT_3D('',#10153,#8293,#8294);
#6859=AXIS2_PLACEMENT_3D('',#10155,#8296,#8297);
#6860=AXIS2_PLACEMENT_3D('',#10156,#8298,#8299);
#6861=AXIS2_PLACEMENT_3D('',#10157,#8300,#8301);
#6862=AXIS2_PLACEMENT_3D('',#10159,#8302,#8303);
#6863=AXIS2_PLACEMENT_3D('',#10162,#8305,#8306);
#6864=AXIS2_PLACEMENT_3D('',#10163,#8307,#8308);
#6865=AXIS2_PLACEMENT_3D('',#10164,#8309,#8310);
#6866=AXIS2_PLACEMENT_3D('',#10166,#8311,#8312);
#6867=AXIS2_PLACEMENT_3D('',#10167,#8313,#8314);
#6868=AXIS2_PLACEMENT_3D('',#10169,#8315,#8316);
#6869=AXIS2_PLACEMENT_3D('',#10171,#8318,#8319);
#6870=AXIS2_PLACEMENT_3D('',#10172,#8320,#8321);
#6871=AXIS2_PLACEMENT_3D('',#10173,#8322,#8323);
#6872=AXIS2_PLACEMENT_3D('',#10176,#8324,#8325);
#6873=AXIS2_PLACEMENT_3D('',#10178,#8326,#8327);
#6874=AXIS2_PLACEMENT_3D('',#10180,#8328,#8329);
#6875=AXIS2_PLACEMENT_3D('',#10182,#8330,#8331);
#6876=AXIS2_PLACEMENT_3D('',#10185,#8333,#8334);
#6877=AXIS2_PLACEMENT_3D('',#10187,#8335,#8336);
#6878=AXIS2_PLACEMENT_3D('',#10189,#8337,#8338);
#6879=AXIS2_PLACEMENT_3D('',#10190,#8339,#8340);
#6880=AXIS2_PLACEMENT_3D('',#10191,#8341,#8342);
#6881=AXIS2_PLACEMENT_3D('',#10192,#8343,#8344);
#6882=AXIS2_PLACEMENT_3D('',#10194,#8346,#8347);
#6883=AXIS2_PLACEMENT_3D('',#10198,#8350,#8351);
#6884=AXIS2_PLACEMENT_3D('',#10202,#8354,#8355);
#6885=AXIS2_PLACEMENT_3D('',#10204,#8357,#8358);
#6886=AXIS2_PLACEMENT_3D('',#10208,#8361,#8362);
#6887=AXIS2_PLACEMENT_3D('',#10212,#8365,#8366);
#6888=AXIS2_PLACEMENT_3D('',#10218,#8370,#8371);
#6889=AXIS2_PLACEMENT_3D('',#10222,#8374,#8375);
#6890=AXIS2_PLACEMENT_3D('',#10226,#8378,#8379);
#6891=AXIS2_PLACEMENT_3D('',#10228,#8381,#8382);
#6892=AXIS2_PLACEMENT_3D('',#10229,#8383,#8384);
#6893=AXIS2_PLACEMENT_3D('',#10230,#8385,#8386);
#6894=AXIS2_PLACEMENT_3D('',#10233,#8387,#8388);
#6895=AXIS2_PLACEMENT_3D('',#10235,#8389,#8390);
#6896=AXIS2_PLACEMENT_3D('',#10237,#8391,#8392);
#6897=AXIS2_PLACEMENT_3D('',#10239,#8393,#8394);
#6898=AXIS2_PLACEMENT_3D('',#10242,#8396,#8397);
#6899=AXIS2_PLACEMENT_3D('',#10244,#8398,#8399);
#6900=AXIS2_PLACEMENT_3D('',#10246,#8400,#8401);
#6901=AXIS2_PLACEMENT_3D('',#10247,#8402,#8403);
#6902=AXIS2_PLACEMENT_3D('',#10248,#8404,#8405);
#6903=AXIS2_PLACEMENT_3D('',#10249,#8406,#8407);
#6904=AXIS2_PLACEMENT_3D('',#10251,#8409,#8410);
#6905=AXIS2_PLACEMENT_3D('',#10255,#8413,#8414);
#6906=AXIS2_PLACEMENT_3D('',#10259,#8417,#8418);
#6907=AXIS2_PLACEMENT_3D('',#10261,#8420,#8421);
#6908=AXIS2_PLACEMENT_3D('',#10265,#8424,#8425);
#6909=AXIS2_PLACEMENT_3D('',#10269,#8428,#8429);
#6910=AXIS2_PLACEMENT_3D('',#10275,#8433,#8434);
#6911=AXIS2_PLACEMENT_3D('',#10279,#8437,#8438);
#6912=AXIS2_PLACEMENT_3D('',#10283,#8441,#8442);
#6913=AXIS2_PLACEMENT_3D('',#10285,#8444,#8445);
#6914=AXIS2_PLACEMENT_3D('',#10286,#8446,#8447);
#6915=AXIS2_PLACEMENT_3D('',#10287,#8448,#8449);
#6916=AXIS2_PLACEMENT_3D('',#10289,#8450,#8451);
#6917=AXIS2_PLACEMENT_3D('',#10292,#8453,#8454);
#6918=AXIS2_PLACEMENT_3D('',#10293,#8455,#8456);
#6919=AXIS2_PLACEMENT_3D('',#10294,#8457,#8458);
#6920=AXIS2_PLACEMENT_3D('',#10296,#8459,#8460);
#6921=AXIS2_PLACEMENT_3D('',#10297,#8461,#8462);
#6922=AXIS2_PLACEMENT_3D('',#10299,#8463,#8464);
#6923=AXIS2_PLACEMENT_3D('',#10301,#8466,#8467);
#6924=AXIS2_PLACEMENT_3D('',#10302,#8468,#8469);
#6925=AXIS2_PLACEMENT_3D('',#10303,#8470,#8471);
#6926=AXIS2_PLACEMENT_3D('',#10306,#8472,#8473);
#6927=AXIS2_PLACEMENT_3D('',#10310,#8475,#8476);
#6928=AXIS2_PLACEMENT_3D('',#10311,#8477,#8478);
#6929=AXIS2_PLACEMENT_3D('',#10312,#8479,#8480);
#6930=AXIS2_PLACEMENT_3D('',#10313,#8481,#8482);
#6931=AXIS2_PLACEMENT_3D('',#10315,#8483,#8484);
#6932=AXIS2_PLACEMENT_3D('',#10319,#8486,#8487);
#6933=AXIS2_PLACEMENT_3D('',#10320,#8488,#8489);
#6934=AXIS2_PLACEMENT_3D('',#10321,#8490,#8491);
#6935=AXIS2_PLACEMENT_3D('',#10324,#8492,#8493);
#6936=AXIS2_PLACEMENT_3D('',#10327,#8495,#8496);
#6937=AXIS2_PLACEMENT_3D('',#10328,#8497,#8498);
#6938=AXIS2_PLACEMENT_3D('',#10329,#8499,#8500);
#6939=AXIS2_PLACEMENT_3D('',#10331,#8501,#8502);
#6940=AXIS2_PLACEMENT_3D('',#10334,#8504,#8505);
#6941=AXIS2_PLACEMENT_3D('',#10335,#8506,#8507);
#6942=AXIS2_PLACEMENT_3D('',#10337,#8508,#8509);
#6943=AXIS2_PLACEMENT_3D('',#10340,#8511,#8512);
#6944=AXIS2_PLACEMENT_3D('',#10341,#8513,#8514);
#6945=AXIS2_PLACEMENT_3D('',#10343,#8515,#8516);
#6946=AXIS2_PLACEMENT_3D('',#10344,#8517,#8518);
#6947=AXIS2_PLACEMENT_3D('',#10346,#8520,#8521);
#6948=AXIS2_PLACEMENT_3D('',#10348,#8522,#8523);
#6949=AXIS2_PLACEMENT_3D('',#10350,#8525,#8526);
#6950=AXIS2_PLACEMENT_3D('',#10352,#8528,#8529);
#6951=AXIS2_PLACEMENT_3D('',#10353,#8530,#8531);
#6952=AXIS2_PLACEMENT_3D('',#10355,#8533,#8534);
#6953=AXIS2_PLACEMENT_3D('',#10356,#8535,#8536);
#6954=AXIS2_PLACEMENT_3D('',#10357,#8537,#8538);
#6955=AXIS2_PLACEMENT_3D('',#10358,#8539,#8540);
#6956=AXIS2_PLACEMENT_3D('',#10359,#8541,#8542);
#6957=AXIS2_PLACEMENT_3D('',#10360,#8543,#8544);
#6958=AXIS2_PLACEMENT_3D('',#10361,#8545,#8546);
#6959=AXIS2_PLACEMENT_3D('',#10362,#8547,#8548);
#6960=AXIS2_PLACEMENT_3D('',#10363,#8549,#8550);
#6961=AXIS2_PLACEMENT_3D('',#10364,#8551,#8552);
#6962=AXIS2_PLACEMENT_3D('',#10365,#8553,#8554);
#6963=AXIS2_PLACEMENT_3D('',#10367,#8555,#8556);
#6964=AXIS2_PLACEMENT_3D('',#10370,#8558,#8559);
#6965=AXIS2_PLACEMENT_3D('',#10371,#8560,#8561);
#6966=AXIS2_PLACEMENT_3D('',#10381,#8566,#8567);
#6967=AXIS2_PLACEMENT_3D('',#10383,#8568,#8569);
#6968=AXIS2_PLACEMENT_3D('',#10385,#8570,#8571);
#6969=AXIS2_PLACEMENT_3D('',#10387,#8572,#8573);
#6970=AXIS2_PLACEMENT_3D('',#10389,#8574,#8575);
#6971=AXIS2_PLACEMENT_3D('',#10391,#8576,#8577);
#6972=AXIS2_PLACEMENT_3D('',#10393,#8578,#8579);
#6973=AXIS2_PLACEMENT_3D('',#10395,#8580,#8581);
#6974=AXIS2_PLACEMENT_3D('',#10396,#8582,#8583);
#6975=AXIS2_PLACEMENT_3D('',#10414,#8592,#8593);
#6976=AXIS2_PLACEMENT_3D('',#10416,#8594,#8595);
#6977=AXIS2_PLACEMENT_3D('',#10418,#8596,#8597);
#6978=AXIS2_PLACEMENT_3D('',#10420,#8598,#8599);
#6979=AXIS2_PLACEMENT_3D('',#10422,#8600,#8601);
#6980=AXIS2_PLACEMENT_3D('',#10424,#8602,#8603);
#6981=AXIS2_PLACEMENT_3D('',#10426,#8604,#8605);
#6982=AXIS2_PLACEMENT_3D('',#10428,#8606,#8607);
#6983=AXIS2_PLACEMENT_3D('',#10429,#8608,#8609);
#6984=AXIS2_PLACEMENT_3D('',#10431,#8611,#8612);
#6985=AXIS2_PLACEMENT_3D('',#10433,#8614,#8615);
#6986=AXIS2_PLACEMENT_3D('',#10435,#8617,#8618);
#6987=AXIS2_PLACEMENT_3D('',#10437,#8620,#8621);
#6988=AXIS2_PLACEMENT_3D('',#10439,#8623,#8624);
#6989=AXIS2_PLACEMENT_3D('',#10441,#8626,#8627);
#6990=AXIS2_PLACEMENT_3D('',#10443,#8629,#8630);
#6991=AXIS2_PLACEMENT_3D('',#10445,#8632,#8633);
#6992=AXIS2_PLACEMENT_3D('',#10456,#8640,#8641);
#6993=AXIS2_PLACEMENT_3D('',#10458,#8643,#8644);
#6994=AXIS2_PLACEMENT_3D('',#10460,#8646,#8647);
#6995=AXIS2_PLACEMENT_3D('',#10468,#8652,#8653);
#6996=AXIS2_PLACEMENT_3D('',#10472,#8656,#8657);
#6997=AXIS2_PLACEMENT_3D('',#10476,#8660,#8661);
#6998=AXIS2_PLACEMENT_3D('',#10480,#8664,#8665);
#6999=AXIS2_PLACEMENT_3D('',#10482,#8667,#8668);
#7000=AXIS2_PLACEMENT_3D('',#10488,#8672,#8673);
#7001=AXIS2_PLACEMENT_3D('',#10491,#8675,#8676);
#7002=AXIS2_PLACEMENT_3D('',#10493,#8677,#8678);
#7003=AXIS2_PLACEMENT_3D('',#10495,#8679,#8680);
#7004=AXIS2_PLACEMENT_3D('',#10497,#8681,#8682);
#7005=AXIS2_PLACEMENT_3D('',#10499,#8683,#8684);
#7006=AXIS2_PLACEMENT_3D('',#10501,#8685,#8686);
#7007=AXIS2_PLACEMENT_3D('',#10503,#8687,#8688);
#7008=AXIS2_PLACEMENT_3D('',#10505,#8689,#8690);
#7009=AXIS2_PLACEMENT_3D('',#10507,#8691,#8692);
#7010=AXIS2_PLACEMENT_3D('',#10508,#8693,#8694);
#7011=AXIS2_PLACEMENT_3D('',#10511,#8696,#8697);
#7012=AXIS2_PLACEMENT_3D('',#10513,#8698,#8699);
#7013=AXIS2_PLACEMENT_3D('',#10515,#8700,#8701);
#7014=AXIS2_PLACEMENT_3D('',#10517,#8702,#8703);
#7015=AXIS2_PLACEMENT_3D('',#10519,#8704,#8705);
#7016=AXIS2_PLACEMENT_3D('',#10521,#8706,#8707);
#7017=AXIS2_PLACEMENT_3D('',#10523,#8708,#8709);
#7018=AXIS2_PLACEMENT_3D('',#10525,#8710,#8711);
#7019=AXIS2_PLACEMENT_3D('',#10527,#8712,#8713);
#7020=AXIS2_PLACEMENT_3D('',#10528,#8714,#8715);
#7021=AXIS2_PLACEMENT_3D('',#10529,#8716,#8717);
#7022=AXIS2_PLACEMENT_3D('',#10531,#8719,#8720);
#7023=AXIS2_PLACEMENT_3D('',#10533,#8722,#8723);
#7024=AXIS2_PLACEMENT_3D('',#10535,#8725,#8726);
#7025=AXIS2_PLACEMENT_3D('',#10537,#8728,#8729);
#7026=AXIS2_PLACEMENT_3D('',#10539,#8731,#8732);
#7027=AXIS2_PLACEMENT_3D('',#10541,#8734,#8735);
#7028=AXIS2_PLACEMENT_3D('',#10543,#8737,#8738);
#7029=AXIS2_PLACEMENT_3D('',#10545,#8740,#8741);
#7030=AXIS2_PLACEMENT_3D('',#10547,#8743,#8744);
#7031=AXIS2_PLACEMENT_3D('',#10548,#8745,#8746);
#7032=AXIS2_PLACEMENT_3D('',#10550,#8747,#8748);
#7033=AXIS2_PLACEMENT_3D('',#10553,#8750,#8751);
#7034=AXIS2_PLACEMENT_3D('',#10554,#8752,#8753);
#7035=AXIS2_PLACEMENT_3D('',#10555,#8754,#8755);
#7036=AXIS2_PLACEMENT_3D('',#10557,#8756,#8757);
#7037=AXIS2_PLACEMENT_3D('',#10558,#8758,#8759);
#7038=AXIS2_PLACEMENT_3D('',#10560,#8760,#8761);
#7039=AXIS2_PLACEMENT_3D('',#10562,#8763,#8764);
#7040=AXIS2_PLACEMENT_3D('',#10564,#8765,#8766);
#7041=AXIS2_PLACEMENT_3D('',#10565,#8767,#8768);
#7042=AXIS2_PLACEMENT_3D('',#10567,#8769,#8770);
#7043=AXIS2_PLACEMENT_3D('',#10569,#8772,#8773);
#7044=AXIS2_PLACEMENT_3D('',#10570,#8774,#8775);
#7045=AXIS2_PLACEMENT_3D('',#10571,#8776,#8777);
#7046=AXIS2_PLACEMENT_3D('',#10572,#8778,#8779);
#7047=AXIS2_PLACEMENT_3D('',#10574,#8780,#8781);
#7048=AXIS2_PLACEMENT_3D('',#10577,#8783,#8784);
#7049=AXIS2_PLACEMENT_3D('',#10578,#8785,#8786);
#7050=AXIS2_PLACEMENT_3D('',#10585,#8789,#8790);
#7051=AXIS2_PLACEMENT_3D('',#10588,#8792,#8793);
#7052=AXIS2_PLACEMENT_3D('',#10589,#8794,#8795);
#7053=AXIS2_PLACEMENT_3D('',#10592,#8797,#8798);
#7054=AXIS2_PLACEMENT_3D('',#10593,#8799,#8800);
#7055=AXIS2_PLACEMENT_3D('',#10599,#8804,#8805);
#7056=AXIS2_PLACEMENT_3D('',#10602,#8807,#8808);
#7057=AXIS2_PLACEMENT_3D('',#10603,#8809,#8810);
#7058=AXIS2_PLACEMENT_3D('',#10607,#8813,#8814);
#7059=AXIS2_PLACEMENT_3D('',#10609,#8816,#8817);
#7060=AXIS2_PLACEMENT_3D('',#10610,#8818,#8819);
#7061=AXIS2_PLACEMENT_3D('',#10611,#8820,#8821);
#7062=AXIS2_PLACEMENT_3D('',#10620,#8826,#8827);
#7063=AXIS2_PLACEMENT_3D('',#10626,#8831,#8832);
#7064=AXIS2_PLACEMENT_3D('',#10630,#8835,#8836);
#7065=AXIS2_PLACEMENT_3D('',#10634,#8839,#8840);
#7066=AXIS2_PLACEMENT_3D('',#10636,#8842,#8843);
#7067=AXIS2_PLACEMENT_3D('',#10637,#8844,#8845);
#7068=AXIS2_PLACEMENT_3D('',#10638,#8846,#8847);
#7069=AXIS2_PLACEMENT_3D('',#10640,#8848,#8849);
#7070=AXIS2_PLACEMENT_3D('',#10643,#8851,#8852);
#7071=AXIS2_PLACEMENT_3D('',#10644,#8853,#8854);
#7072=AXIS2_PLACEMENT_3D('',#10651,#8857,#8858);
#7073=AXIS2_PLACEMENT_3D('',#10654,#8860,#8861);
#7074=AXIS2_PLACEMENT_3D('',#10655,#8862,#8863);
#7075=AXIS2_PLACEMENT_3D('',#10658,#8865,#8866);
#7076=AXIS2_PLACEMENT_3D('',#10659,#8867,#8868);
#7077=AXIS2_PLACEMENT_3D('',#10665,#8872,#8873);
#7078=AXIS2_PLACEMENT_3D('',#10668,#8875,#8876);
#7079=AXIS2_PLACEMENT_3D('',#10669,#8877,#8878);
#7080=AXIS2_PLACEMENT_3D('',#10673,#8881,#8882);
#7081=AXIS2_PLACEMENT_3D('',#10675,#8884,#8885);
#7082=AXIS2_PLACEMENT_3D('',#10676,#8886,#8887);
#7083=AXIS2_PLACEMENT_3D('',#10677,#8888,#8889);
#7084=AXIS2_PLACEMENT_3D('',#10679,#8890,#8891);
#7085=AXIS2_PLACEMENT_3D('',#10682,#8893,#8894);
#7086=AXIS2_PLACEMENT_3D('',#10683,#8895,#8896);
#7087=AXIS2_PLACEMENT_3D('',#10697,#8903,#8904);
#7088=AXIS2_PLACEMENT_3D('',#10699,#8905,#8906);
#7089=AXIS2_PLACEMENT_3D('',#10700,#8907,#8908);
#7090=AXIS2_PLACEMENT_3D('',#10714,#8916,#8917);
#7091=AXIS2_PLACEMENT_3D('',#10718,#8920,#8921);
#7092=AXIS2_PLACEMENT_3D('',#10722,#8924,#8925);
#7093=AXIS2_PLACEMENT_3D('',#10726,#8928,#8929);
#7094=AXIS2_PLACEMENT_3D('',#10738,#8936,#8937);
#7095=AXIS2_PLACEMENT_3D('',#10742,#8940,#8941);
#7096=AXIS2_PLACEMENT_3D('',#10743,#8942,#8943);
#7097=AXIS2_PLACEMENT_3D('',#10745,#8945,#8946);
#7098=AXIS2_PLACEMENT_3D('',#10747,#8947,#8948);
#7099=AXIS2_PLACEMENT_3D('',#10748,#8949,#8950);
#7100=AXIS2_PLACEMENT_3D('',#10750,#8952,#8953);
#7101=AXIS2_PLACEMENT_3D('',#10753,#8955,#8956);
#7102=AXIS2_PLACEMENT_3D('',#10755,#8957,#8958);
#7103=AXIS2_PLACEMENT_3D('',#10756,#8959,#8960);
#7104=AXIS2_PLACEMENT_3D('',#10757,#8961,#8962);
#7105=AXIS2_PLACEMENT_3D('',#10759,#8964,#8965);
#7106=AXIS2_PLACEMENT_3D('',#10761,#8967,#8968);
#7107=AXIS2_PLACEMENT_3D('',#10763,#8970,#8971);
#7108=AXIS2_PLACEMENT_3D('',#10764,#8972,#8973);
#7109=AXIS2_PLACEMENT_3D('',#10766,#8974,#8975);
#7110=AXIS2_PLACEMENT_3D('',#10769,#8977,#8978);
#7111=AXIS2_PLACEMENT_3D('',#10770,#8979,#8980);
#7112=AXIS2_PLACEMENT_3D('',#10777,#8983,#8984);
#7113=AXIS2_PLACEMENT_3D('',#10780,#8986,#8987);
#7114=AXIS2_PLACEMENT_3D('',#10781,#8988,#8989);
#7115=AXIS2_PLACEMENT_3D('',#10784,#8991,#8992);
#7116=AXIS2_PLACEMENT_3D('',#10785,#8993,#8994);
#7117=AXIS2_PLACEMENT_3D('',#10791,#8998,#8999);
#7118=AXIS2_PLACEMENT_3D('',#10794,#9001,#9002);
#7119=AXIS2_PLACEMENT_3D('',#10795,#9003,#9004);
#7120=AXIS2_PLACEMENT_3D('',#10799,#9007,#9008);
#7121=AXIS2_PLACEMENT_3D('',#10801,#9010,#9011);
#7122=AXIS2_PLACEMENT_3D('',#10802,#9012,#9013);
#7123=AXIS2_PLACEMENT_3D('',#10803,#9014,#9015);
#7124=AXIS2_PLACEMENT_3D('',#10805,#9016,#9017);
#7125=AXIS2_PLACEMENT_3D('',#10808,#9019,#9020);
#7126=AXIS2_PLACEMENT_3D('',#10809,#9021,#9022);
#7127=AXIS2_PLACEMENT_3D('',#10816,#9025,#9026);
#7128=AXIS2_PLACEMENT_3D('',#10819,#9028,#9029);
#7129=AXIS2_PLACEMENT_3D('',#10820,#9030,#9031);
#7130=AXIS2_PLACEMENT_3D('',#10823,#9033,#9034);
#7131=AXIS2_PLACEMENT_3D('',#10824,#9035,#9036);
#7132=AXIS2_PLACEMENT_3D('',#10830,#9040,#9041);
#7133=AXIS2_PLACEMENT_3D('',#10833,#9043,#9044);
#7134=AXIS2_PLACEMENT_3D('',#10834,#9045,#9046);
#7135=AXIS2_PLACEMENT_3D('',#10838,#9049,#9050);
#7136=AXIS2_PLACEMENT_3D('',#10840,#9052,#9053);
#7137=AXIS2_PLACEMENT_3D('',#10841,#9054,#9055);
#7138=AXIS2_PLACEMENT_3D('',#10842,#9056,#9057);
#7139=AXIS2_PLACEMENT_3D('',#10843,#9058,#9059);
#7140=AXIS2_PLACEMENT_3D('',#10844,#9060,#9061);
#7141=AXIS2_PLACEMENT_3D('',#10845,#9062,#9063);
#7142=AXIS2_PLACEMENT_3D('',#10846,#9064,#9065);
#7143=AXIS2_PLACEMENT_3D('',#10847,#9066,#9067);
#7144=AXIS2_PLACEMENT_3D('',#10848,#9068,#9069);
#7145=AXIS2_PLACEMENT_3D('',#10849,#9070,#9071);
#7146=AXIS2_PLACEMENT_3D('',#10852,#9072,#9073);
#7147=AXIS2_PLACEMENT_3D('',#10853,#9074,#9075);
#7148=AXIS2_PLACEMENT_3D('',#10854,#9076,#9077);
#7149=AXIS2_PLACEMENT_3D('',#10858,#9079,#9080);
#7150=AXIS2_PLACEMENT_3D('',#10859,#9081,#9082);
#7151=AXIS2_PLACEMENT_3D('',#10860,#9083,#9084);
#7152=AXIS2_PLACEMENT_3D('',#10861,#9085,#9086);
#7153=AXIS2_PLACEMENT_3D('',#10862,#9087,#9088);
#7154=AXIS2_PLACEMENT_3D('',#10864,#9089,#9090);
#7155=AXIS2_PLACEMENT_3D('',#10867,#9092,#9093);
#7156=AXIS2_PLACEMENT_3D('',#10868,#9094,#9095);
#7157=AXIS2_PLACEMENT_3D('',#10869,#9096,#9097);
#7158=AXIS2_PLACEMENT_3D('',#10870,#9098,#9099);
#7159=AXIS2_PLACEMENT_3D('',#10871,#9100,#9101);
#7160=AXIS2_PLACEMENT_3D('',#10873,#9102,#9103);
#7161=AXIS2_PLACEMENT_3D('',#10876,#9105,#9106);
#7162=AXIS2_PLACEMENT_3D('',#10877,#9107,#9108);
#7163=AXIS2_PLACEMENT_3D('',#10879,#9109,#9110);
#7164=AXIS2_PLACEMENT_3D('',#10880,#9111,#9112);
#7165=AXIS2_PLACEMENT_3D('',#10882,#9113,#9114);
#7166=AXIS2_PLACEMENT_3D('',#10883,#9115,#9116);
#7167=AXIS2_PLACEMENT_3D('',#10885,#9118,#9119);
#7168=AXIS2_PLACEMENT_3D('',#10886,#9120,#9121);
#7169=AXIS2_PLACEMENT_3D('',#10889,#9122,#9123);
#7170=AXIS2_PLACEMENT_3D('',#10890,#9124,#9125);
#7171=AXIS2_PLACEMENT_3D('',#10891,#9126,#9127);
#7172=AXIS2_PLACEMENT_3D('',#10895,#9129,#9130);
#7173=AXIS2_PLACEMENT_3D('',#10896,#9131,#9132);
#7174=AXIS2_PLACEMENT_3D('',#10897,#9133,#9134);
#7175=AXIS2_PLACEMENT_3D('',#10898,#9135,#9136);
#7176=AXIS2_PLACEMENT_3D('',#10899,#9137,#9138);
#7177=AXIS2_PLACEMENT_3D('',#10901,#9139,#9140);
#7178=AXIS2_PLACEMENT_3D('',#10904,#9142,#9143);
#7179=AXIS2_PLACEMENT_3D('',#10905,#9144,#9145);
#7180=AXIS2_PLACEMENT_3D('',#10906,#9146,#9147);
#7181=AXIS2_PLACEMENT_3D('',#10907,#9148,#9149);
#7182=AXIS2_PLACEMENT_3D('',#10908,#9150,#9151);
#7183=AXIS2_PLACEMENT_3D('',#10909,#9152,#9153);
#7184=AXIS2_PLACEMENT_3D('',#10910,#9154,#9155);
#7185=AXIS2_PLACEMENT_3D('',#10911,#9156,#9157);
#7186=AXIS2_PLACEMENT_3D('',#10912,#9158,#9159);
#7187=AXIS2_PLACEMENT_3D('',#10913,#9160,#9161);
#7188=AXIS2_PLACEMENT_3D('',#10915,#9162,#9163);
#7189=AXIS2_PLACEMENT_3D('',#10918,#9165,#9166);
#7190=AXIS2_PLACEMENT_3D('',#10919,#9167,#9168);
#7191=AXIS2_PLACEMENT_3D('',#10921,#9169,#9170);
#7192=AXIS2_PLACEMENT_3D('',#10922,#9171,#9172);
#7193=AXIS2_PLACEMENT_3D('',#10929,#9175,#9176);
#7194=AXIS2_PLACEMENT_3D('',#10930,#9177,#9178);
#7195=AXIS2_PLACEMENT_3D('',#10932,#9179,#9180);
#7196=AXIS2_PLACEMENT_3D('',#10934,#9181,#9182);
#7197=AXIS2_PLACEMENT_3D('',#10936,#9183,#9184);
#7198=AXIS2_PLACEMENT_3D('',#10938,#9185,#9186);
#7199=AXIS2_PLACEMENT_3D('',#10939,#9187,#9188);
#7200=AXIS2_PLACEMENT_3D('',#10941,#9189,#9190);
#7201=AXIS2_PLACEMENT_3D('',#10943,#9192,#9193);
#7202=AXIS2_PLACEMENT_3D('',#10945,#9194,#9195);
#7203=AXIS2_PLACEMENT_3D('',#10947,#9197,#9198);
#7204=AXIS2_PLACEMENT_3D('',#10949,#9199,#9200);
#7205=AXIS2_PLACEMENT_3D('',#10951,#9202,#9203);
#7206=AXIS2_PLACEMENT_3D('',#10953,#9204,#9205);
#7207=AXIS2_PLACEMENT_3D('',#10955,#9207,#9208);
#7208=AXIS2_PLACEMENT_3D('',#10957,#9209,#9210);
#7209=AXIS2_PLACEMENT_3D('',#10959,#9212,#9213);
#7210=AXIS2_PLACEMENT_3D('',#10965,#9217,#9218);
#7211=AXIS2_PLACEMENT_3D('',#10967,#9219,#9220);
#7212=AXIS2_PLACEMENT_3D('',#10969,#9222,#9223);
#7213=AXIS2_PLACEMENT_3D('',#10972,#9225,#9226);
#7214=AXIS2_PLACEMENT_3D('',#10973,#9227,#9228);
#7215=AXIS2_PLACEMENT_3D('',#10975,#9230,#9231);
#7216=AXIS2_PLACEMENT_3D('',#10976,#9232,#9233);
#7217=AXIS2_PLACEMENT_3D('',#10977,#9234,#9235);
#7218=AXIS2_PLACEMENT_3D('',#10978,#9236,#9237);
#7219=AXIS2_PLACEMENT_3D('',#10980,#9238,#9239);
#7220=AXIS2_PLACEMENT_3D('',#10983,#9241,#9242);
#7221=AXIS2_PLACEMENT_3D('',#10984,#9243,#9244);
#7222=AXIS2_PLACEMENT_3D('',#10986,#9245,#9246);
#7223=AXIS2_PLACEMENT_3D('',#10987,#9247,#9248);
#7224=AXIS2_PLACEMENT_3D('',#10989,#9249,#9250);
#7225=AXIS2_PLACEMENT_3D('',#10990,#9251,#9252);
#7226=AXIS2_PLACEMENT_3D('',#10992,#9254,#9255);
#7227=AXIS2_PLACEMENT_3D('',#10993,#9256,#9257);
#7228=AXIS2_PLACEMENT_3D('',#10995,#9258,#9259);
#7229=AXIS2_PLACEMENT_3D('',#10998,#9261,#9262);
#7230=AXIS2_PLACEMENT_3D('',#10999,#9263,#9264);
#7231=AXIS2_PLACEMENT_3D('',#11001,#9265,#9266);
#7232=AXIS2_PLACEMENT_3D('',#11002,#9267,#9268);
#7233=AXIS2_PLACEMENT_3D('',#11004,#9269,#9270);
#7234=AXIS2_PLACEMENT_3D('',#11005,#9271,#9272);
#7235=AXIS2_PLACEMENT_3D('',#11007,#9274,#9275);
#7236=AXIS2_PLACEMENT_3D('',#11008,#9276,#9277);
#7237=AXIS2_PLACEMENT_3D('',#11010,#9278,#9279);
#7238=AXIS2_PLACEMENT_3D('',#11013,#9281,#9282);
#7239=AXIS2_PLACEMENT_3D('',#11014,#9283,#9284);
#7240=AXIS2_PLACEMENT_3D('',#11015,#9285,#9286);
#7241=AXIS2_PLACEMENT_3D('',#11016,#9287,#9288);
#7242=AXIS2_PLACEMENT_3D('',#11017,#9289,#9290);
#7243=AXIS2_PLACEMENT_3D('',#11018,#9291,#9292);
#7244=AXIS2_PLACEMENT_3D('',#11019,#9293,#9294);
#7245=AXIS2_PLACEMENT_3D('',#11020,#9295,#9296);
#7246=AXIS2_PLACEMENT_3D('',#11021,#9297,#9298);
#7247=AXIS2_PLACEMENT_3D('',#11022,#9299,#9300);
#7248=AXIS2_PLACEMENT_3D('',#11023,#9301,#9302);
#7249=AXIS2_PLACEMENT_3D('',#11024,#9303,#9304);
#7250=AXIS2_PLACEMENT_3D('',#11025,#9305,#9306);
#7251=AXIS2_PLACEMENT_3D('',#11026,#9307,#9308);
#7252=AXIS2_PLACEMENT_3D('',#11027,#9309,#9310);
#7253=AXIS2_PLACEMENT_3D('',#11028,#9311,#9312);
#7254=AXIS2_PLACEMENT_3D('',#11029,#9313,#9314);
#7255=AXIS2_PLACEMENT_3D('',#11030,#9315,#9316);
#7256=AXIS2_PLACEMENT_3D('',#11031,#9317,#9318);
#7257=AXIS2_PLACEMENT_3D('',#11032,#9319,#9320);
#7258=AXIS2_PLACEMENT_3D('',#11033,#9321,#9322);
#7259=AXIS2_PLACEMENT_3D('',#11034,#9323,#9324);
#7260=DIRECTION('axis',(0.,0.,1.));
#7261=DIRECTION('refdir',(1.,0.,0.));
#7262=DIRECTION('axis',(0.,0.,1.));
#7263=DIRECTION('refdir',(1.,0.,0.));
#7264=DIRECTION('center_axis',(0.,0.,1.));
#7265=DIRECTION('ref_axis',(1.,1.37975427514318E-9,0.));
#7266=DIRECTION('center_axis',(6.39458016332861E-18,1.10411609048463E-17,
1.));
#7267=DIRECTION('ref_axis',(1.,1.37975427514318E-9,0.));
#7268=DIRECTION('',(0.,0.,-1.));
#7269=DIRECTION('center_axis',(0.,0.,1.));
#7270=DIRECTION('ref_axis',(1.,1.37975427514318E-9,0.));
#7271=DIRECTION('center_axis',(4.13029399042097E-17,0.,1.));
#7272=DIRECTION('ref_axis',(1.,0.,-4.13029399042097E-17));
#7273=DIRECTION('center_axis',(-3.04809470411818E-27,2.64338815530979E-17,
1.));
#7274=DIRECTION('ref_axis',(1.,-4.29586510583046E-10,0.));
#7275=DIRECTION('',(-4.13029399042097E-17,0.,-1.));
#7276=DIRECTION('center_axis',(-5.28677630773884E-17,-1.0843360466812E-26,
-1.));
#7277=DIRECTION('ref_axis',(1.,2.50000086925735E-10,-5.28677630773884E-17));
#7278=DIRECTION('center_axis',(-5.28677630773884E-17,-1.0843360466812E-26,
-1.));
#7279=DIRECTION('ref_axis',(1.,2.50000086925735E-10,-5.28677630773884E-17));
#7280=DIRECTION('center_axis',(-1.70140119462979E-16,0.,-1.));
#7281=DIRECTION('ref_axis',(-1.,0.,1.70140119462979E-16));
#7282=DIRECTION('center_axis',(-9.76996261870523E-16,-9.7699626151362E-16,
-1.));
#7283=DIRECTION('ref_axis',(1.,-1.60206417040051E-10,-9.76996261670138E-16));
#7284=DIRECTION('',(-0.86602541098055,1.0605752475376E-16,0.49999998753597));
#7285=DIRECTION('center_axis',(1.70140119462979E-16,0.,1.));
#7286=DIRECTION('ref_axis',(1.,0.,-1.70140119462979E-16));
#7287=DIRECTION('center_axis',(0.,0.,1.));
#7288=DIRECTION('ref_axis',(-1.,-1.60206710118277E-10,0.));
#7289=DIRECTION('',(0.86602541098055,1.0605752475376E-16,-0.49999998753597));
#7290=DIRECTION('center_axis',(0.,0.,1.));
#7291=DIRECTION('ref_axis',(-1.,-1.60206710118277E-10,0.));
#7292=DIRECTION('center_axis',(0.,0.,-1.));
#7293=DIRECTION('ref_axis',(-1.,0.,0.));
#7294=DIRECTION('center_axis',(0.,0.,-1.));
#7295=DIRECTION('ref_axis',(-1.,0.,0.));
#7296=DIRECTION('',(0.,0.,1.));
#7297=DIRECTION('center_axis',(0.,0.,-1.));
#7298=DIRECTION('ref_axis',(-1.,0.,0.));
#7299=DIRECTION('',(0.,0.,1.));
#7300=DIRECTION('center_axis',(0.,0.,-1.));
#7301=DIRECTION('ref_axis',(-1.,0.,0.));
#7302=DIRECTION('center_axis',(2.84990285479818E-18,3.64291930135101E-18,
1.));
#7303=DIRECTION('ref_axis',(0.,-1.,3.64291930135101E-18));
#7304=DIRECTION('center_axis',(-2.16840434497101E-17,0.,-1.));
#7305=DIRECTION('ref_axis',(-1.,0.,2.16840434497101E-17));
#7306=DIRECTION('center_axis',(-2.84990285479818E-18,-3.64291930135101E-18,
1.));
#7307=DIRECTION('ref_axis',(0.,-1.,-3.64291930135101E-18));
#7308=DIRECTION('center_axis',(0.,0.,-1.));
#7309=DIRECTION('ref_axis',(-1.,0.,0.));
#7310=DIRECTION('center_axis',(-2.16840434497101E-17,0.,-1.));
#7311=DIRECTION('ref_axis',(-1.,0.,2.16840434497101E-17));
#7312=DIRECTION('center_axis',(-2.16840434497101E-17,0.,-1.));
#7313=DIRECTION('ref_axis',(-1.,0.,2.16840434497101E-17));
#7314=DIRECTION('',(-2.16840434497101E-17,0.,-1.));
#7315=DIRECTION('center_axis',(0.,0.,-1.));
#7316=DIRECTION('ref_axis',(-1.,0.,0.));
#7317=DIRECTION('',(0.,0.,-1.));
#7318=DIRECTION('center_axis',(0.,0.,-1.));
#7319=DIRECTION('ref_axis',(-1.,0.,0.));
#7320=DIRECTION('center_axis',(-6.27288400105048E-18,-2.92734586715581E-18,
1.));
#7321=DIRECTION('ref_axis',(1.,-1.25733582200228E-51,6.27288400105048E-18));
#7322=DIRECTION('center_axis',(-3.46944695195361E-16,0.,1.));
#7323=DIRECTION('ref_axis',(1.,0.,3.46944695195361E-16));
#7324=DIRECTION('center_axis',(-3.46944695195361E-16,0.,1.));
#7325=DIRECTION('ref_axis',(1.,0.,3.46944695195361E-16));
#7326=DIRECTION('center_axis',(-3.46944695195362E-16,0.,1.));
#7327=DIRECTION('ref_axis',(1.,0.,3.46944695195362E-16));
#7328=DIRECTION('center_axis',(-3.46944695195361E-16,0.,1.));
#7329=DIRECTION('ref_axis',(1.,0.,3.46944695195361E-16));
#7330=DIRECTION('center_axis',(-3.46944695195361E-16,0.,1.));
#7331=DIRECTION('ref_axis',(1.,0.,3.46944695195361E-16));
#7332=DIRECTION('center_axis',(-3.46944695195362E-16,0.,1.));
#7333=DIRECTION('ref_axis',(1.,0.,3.46944695195362E-16));
#7334=DIRECTION('center_axis',(0.,0.,-1.));
#7335=DIRECTION('ref_axis',(-1.,0.,0.));
#7336=DIRECTION('center_axis',(6.27288400105048E-18,2.92734586715581E-18,
1.));
#7337=DIRECTION('ref_axis',(1.,-1.25733582200228E-51,-6.27288400105048E-18));
#7338=DIRECTION('center_axis',(-3.46944695195361E-16,0.,1.));
#7339=DIRECTION('ref_axis',(1.,0.,3.46944695195361E-16));
#7340=DIRECTION('center_axis',(-3.46944695195361E-16,0.,1.));
#7341=DIRECTION('ref_axis',(1.,0.,3.46944695195361E-16));
#7342=DIRECTION('center_axis',(-3.46944695195362E-16,0.,1.));
#7343=DIRECTION('ref_axis',(1.,0.,3.46944695195362E-16));
#7344=DIRECTION('center_axis',(-3.46944695195361E-16,0.,1.));
#7345=DIRECTION('ref_axis',(1.,0.,3.46944695195361E-16));
#7346=DIRECTION('center_axis',(-3.46944695195361E-16,0.,1.));
#7347=DIRECTION('ref_axis',(1.,0.,3.46944695195361E-16));
#7348=DIRECTION('center_axis',(-3.46944695195362E-16,0.,1.));
#7349=DIRECTION('ref_axis',(1.,0.,3.46944695195362E-16));
#7350=DIRECTION('center_axis',(0.,0.,-1.));
#7351=DIRECTION('ref_axis',(-1.,0.,0.));
#7352=DIRECTION('center_axis',(0.,0.,-1.));
#7353=DIRECTION('ref_axis',(-1.,0.,0.));
#7354=DIRECTION('center_axis',(0.,0.,-1.));
#7355=DIRECTION('ref_axis',(-1.,0.,0.));
#7356=DIRECTION('',(0.,0.,1.));
#7357=DIRECTION('center_axis',(-3.46944695195362E-16,0.,1.));
#7358=DIRECTION('ref_axis',(1.,0.,3.46944695195362E-16));
#7359=DIRECTION('',(-3.46944695195362E-16,0.,1.));
#7360=DIRECTION('center_axis',(-3.46944695195361E-16,0.,1.));
#7361=DIRECTION('ref_axis',(1.,0.,3.46944695195361E-16));
#7362=DIRECTION('',(-3.46944695195361E-16,0.,1.));
#7363=DIRECTION('center_axis',(-3.46944695195361E-16,0.,1.));
#7364=DIRECTION('ref_axis',(1.,0.,3.46944695195361E-16));
#7365=DIRECTION('',(-3.46944695195361E-16,0.,1.));
#7366=DIRECTION('center_axis',(-3.46944695195362E-16,0.,1.));
#7367=DIRECTION('ref_axis',(1.,0.,3.46944695195362E-16));
#7368=DIRECTION('',(-3.46944695195362E-16,0.,1.));
#7369=DIRECTION('center_axis',(-3.46944695195361E-16,0.,1.));
#7370=DIRECTION('ref_axis',(1.,0.,3.46944695195361E-16));
#7371=DIRECTION('',(-3.46944695195361E-16,0.,1.));
#7372=DIRECTION('center_axis',(-3.46944695195361E-16,0.,1.));
#7373=DIRECTION('ref_axis',(1.,0.,3.46944695195361E-16));
#7374=DIRECTION('',(-3.46944695195361E-16,0.,1.));
#7375=DIRECTION('center_axis',(0.,0.,-1.));
#7376=DIRECTION('ref_axis',(-1.,0.,0.));
#7377=DIRECTION('',(0.,0.,1.));
#7378=DIRECTION('center_axis',(0.,0.,-1.));
#7379=DIRECTION('ref_axis',(-1.,0.,0.));
#7380=DIRECTION('center_axis',(-6.39458016332861E-18,-1.10411609048463E-17,
1.));
#7381=DIRECTION('ref_axis',(0.,-1.,-1.10411609048463E-17));
#7382=DIRECTION('center_axis',(6.39458016332861E-18,1.10411609048463E-17,
1.));
#7383=DIRECTION('ref_axis',(0.,-1.,1.10411609048463E-17));
#7384=DIRECTION('axis',(0.,0.,1.));
#7385=DIRECTION('refdir',(1.,0.,0.));
#7386=DIRECTION('center_axis',(1.,4.17203717831812E-9,1.01277540341552E-17));
#7387=DIRECTION('ref_axis',(-4.1720371751696E-9,1.,0.));
#7388=DIRECTION('center_axis',(1.,4.17203717831812E-9,1.01277540341552E-17));
#7389=DIRECTION('ref_axis',(-4.17203717831812E-9,1.,-1.69634196247466E-42));
#7390=DIRECTION('center_axis',(8.36866394062756E-10,1.,-8.36884415538179E-10));
#7391=DIRECTION('ref_axis',(-7.96162761077703E-7,8.36885081819775E-10,0.999999999999683));
#7392=DIRECTION('center_axis',(1.,4.17203717831812E-9,1.01277540341552E-17));
#7393=DIRECTION('ref_axis',(-4.17203717831812E-9,1.,-1.69634196247466E-42));
#7394=DIRECTION('center_axis',(8.36869948186391E-10,1.,8.36891441629708E-10));
#7395=DIRECTION('ref_axis',(-0.999999999999707,8.36870588457614E-10,-7.65059166582913E-7));
#7396=DIRECTION('center_axis',(1.,-4.17203708245403E-9,6.73890284431642E-18));
#7397=DIRECTION('ref_axis',(-4.1720370750894E-9,-1.,5.66553889764798E-16));
#7398=DIRECTION('center_axis',(1.,-4.17203708245403E-9,6.73890284431642E-18));
#7399=DIRECTION('ref_axis',(4.17203708245403E-9,1.,-1.23465054354127E-43));
#7400=DIRECTION('center_axis',(-1.,4.17203697154146E-9,4.27849718847752E-19));
#7401=DIRECTION('ref_axis',(-4.27008851558771E-17,-5.34839554841822E-9,
1.));
#7402=DIRECTION('center_axis',(1.,0.,-3.33600668457079E-17));
#7403=DIRECTION('ref_axis',(-3.33600668457079E-17,0.,-1.));
#7404=DIRECTION('center_axis',(1.,0.,-3.33600668457079E-17));
#7405=DIRECTION('ref_axis',(-3.33600668457079E-17,0.,-1.));
#7406=DIRECTION('center_axis',(1.,0.,0.));
#7407=DIRECTION('ref_axis',(0.,-4.64793894161955E-10,-1.));
#7408=DIRECTION('',(-1.,0.,3.33600668457079E-17));
#7409=DIRECTION('center_axis',(-1.,1.53144334479515E-17,1.9842828066192E-17));
#7410=DIRECTION('ref_axis',(1.9842828066192E-17,0.,1.));
#7411=DIRECTION('center_axis',(1.,0.,0.));
#7412=DIRECTION('ref_axis',(0.,0.,-1.));
#7413=DIRECTION('center_axis',(1.,-4.17203727418451E-9,-1.07069540457721E-17));
#7414=DIRECTION('ref_axis',(4.1720372752498E-9,1.,0.));
#7415=DIRECTION('center_axis',(-8.36866342496331E-10,1.,-8.36883936494317E-10));
#7416=DIRECTION('ref_axis',(0.999999999999707,8.36866982761818E-10,7.65059174657239E-7));
#7417=DIRECTION('center_axis',(1.,-4.17203727418451E-9,-1.07069540457721E-17));
#7418=DIRECTION('ref_axis',(4.17203727418451E-9,1.,1.45967462857766E-42));
#7419=DIRECTION('center_axis',(-8.36844869453255E-10,1.,8.36865935422119E-10));
#7420=DIRECTION('ref_axis',(9.00645352209864E-7,8.36866689122222E-10,-0.999999999999595));
#7421=DIRECTION('center_axis',(1.,0.,0.));
#7422=DIRECTION('ref_axis',(0.,0.,-1.));
#7423=DIRECTION('',(1.,0.,0.));
#7424=DIRECTION('center_axis',(1.,0.,0.));
#7425=DIRECTION('ref_axis',(0.,-4.29586394988857E-10,-1.));
#7426=DIRECTION('center_axis',(1.,0.,0.));
#7427=DIRECTION('ref_axis',(0.,-4.29586394988857E-10,-1.));
#7428=DIRECTION('center_axis',(1.,4.17203725971588E-9,2.0031116033889E-18));
#7429=DIRECTION('ref_axis',(4.1720372752498E-9,-1.,5.66553889764798E-16));
#7430=DIRECTION('center_axis',(1.,4.17203725971588E-9,2.0031116033889E-18));
#7431=DIRECTION('ref_axis',(-4.17203725971588E-9,1.,5.39459847610519E-43));
#7432=DIRECTION('center_axis',(1.,1.53144334479515E-17,-1.9842828066192E-17));
#7433=DIRECTION('ref_axis',(-1.9842828066192E-17,0.,-1.));
#7434=DIRECTION('center_axis',(1.,0.,0.));
#7435=DIRECTION('ref_axis',(0.,0.,-1.));
#7436=DIRECTION('center_axis',(1.,6.36556116938371E-17,1.00386354793954E-17));
#7437=DIRECTION('ref_axis',(-6.3655612933414E-17,1.,0.));
#7438=DIRECTION('center_axis',(1.00386354793954E-17,1.22464679914735E-16,
-1.));
#7439=DIRECTION('ref_axis',(6.36556105223495E-17,-1.,-1.22464679914735E-16));
#7440=DIRECTION('center_axis',(1.,1.35504238326755E-16,2.34999225611352E-17));
#7441=DIRECTION('ref_axis',(-1.35504238326755E-16,1.,1.40763492406121E-49));
#7442=DIRECTION('center_axis',(1.,1.35504238326755E-16,2.34999225611352E-17));
#7443=DIRECTION('ref_axis',(-1.35504238326755E-16,1.,1.40763492406121E-49));
#7444=DIRECTION('center_axis',(1.,0.,0.));
#7445=DIRECTION('ref_axis',(0.,0.,-1.));
#7446=DIRECTION('center_axis',(-1.,0.,0.));
#7447=DIRECTION('ref_axis',(0.,-6.60206605267583E-10,1.));
#7448=DIRECTION('center_axis',(-1.,0.,0.));
#7449=DIRECTION('ref_axis',(0.,-6.60206605267583E-10,1.));
#7450=DIRECTION('',(1.,0.,0.));
#7451=DIRECTION('center_axis',(1.,0.,0.));
#7452=DIRECTION('ref_axis',(0.,0.,-1.));
#7453=DIRECTION('',(-1.,0.,0.));
#7454=DIRECTION('center_axis',(1.,0.,0.));
#7455=DIRECTION('ref_axis',(0.,0.,-1.));
#7456=DIRECTION('center_axis',(1.,1.18552772674719E-16,-1.97711088800387E-17));
#7457=DIRECTION('ref_axis',(-1.18552772074394E-16,1.,0.));
#7458=DIRECTION('center_axis',(-1.,0.,0.));
#7459=DIRECTION('ref_axis',(0.,-2.05103586755523E-10,1.));
#7460=DIRECTION('center_axis',(-1.97711088800387E-17,1.22464679914735E-16,
-1.));
#7461=DIRECTION('ref_axis',(1.18552771796194E-16,-1.,-1.22464679914735E-16));
#7462=DIRECTION('center_axis',(-1.,0.,0.));
#7463=DIRECTION('ref_axis',(0.,-2.05103586755523E-10,1.));
#7464=DIRECTION('center_axis',(-1.,2.92206431305708E-17,3.78610282642285E-17));
#7465=DIRECTION('ref_axis',(3.78610282642285E-17,0.,1.));
#7466=DIRECTION('center_axis',(1.,1.20795004338275E-8,6.525328094131E-17));
#7467=DIRECTION('ref_axis',(-1.20795004338275E-8,1.,4.44135209129409E-41));
#7468=DIRECTION('center_axis',(1.,-1.20794999078492E-8,-6.65136044666218E-17));
#7469=DIRECTION('ref_axis',(1.20794999078492E-8,1.,-3.20659696454606E-41));
#7470=DIRECTION('center_axis',(1.,0.,0.));
#7471=DIRECTION('ref_axis',(0.,0.,-1.));
#7472=DIRECTION('center_axis',(1.,0.,0.));
#7473=DIRECTION('ref_axis',(0.,0.,-1.));
#7474=DIRECTION('',(-1.,0.,0.));
#7475=DIRECTION('center_axis',(1.,-1.20794999078492E-8,-6.65136044666218E-17));
#7476=DIRECTION('ref_axis',(-1.20794999243885E-8,-1.,-5.21792575105832E-12));
#7477=DIRECTION('center_axis',(-3.90112644891662E-10,-1.,-3.90117034748036E-10));
#7478=DIRECTION('ref_axis',(-7.96162782272821E-7,3.90117345341081E-10,-0.999999999999683));
#7479=DIRECTION('center_axis',(1.,-1.20794992145421E-8,-4.8381018443521E-19));
#7480=DIRECTION('ref_axis',(1.48029741503464E-16,1.78300800621899E-8,-1.));
#7481=DIRECTION('center_axis',(-3.90083830404282E-10,-1.,3.90119162273478E-10));
#7482=DIRECTION('ref_axis',(-0.999999999999707,3.90084128868405E-10,7.65059156489968E-7));
#7483=DIRECTION('center_axis',(1.,1.20795004338275E-8,6.525328094131E-17));
#7484=DIRECTION('ref_axis',(-1.20795004609008E-8,1.,0.));
#7485=DIRECTION('center_axis',(1.,1.20795004338275E-8,6.525328094131E-17));
#7486=DIRECTION('ref_axis',(-1.20795004338275E-8,1.,4.44135209129409E-41));
#7487=DIRECTION('center_axis',(1.,2.92206431305708E-17,-3.78610282642285E-17));
#7488=DIRECTION('ref_axis',(-3.78610282642285E-17,0.,-1.));
#7489=DIRECTION('center_axis',(1.,-1.20794999071527E-8,2.28224857621035E-17));
#7490=DIRECTION('ref_axis',(1.20794999071527E-8,1.,-1.89856639006012E-41));
#7491=DIRECTION('center_axis',(1.,1.20794999172425E-8,-1.59545740616835E-17));
#7492=DIRECTION('ref_axis',(-1.20794999172425E-8,1.,2.99570552288603E-42));
#7493=DIRECTION('center_axis',(1.,0.,-1.15648231731787E-16));
#7494=DIRECTION('ref_axis',(-1.15648231731787E-16,0.,-1.));
#7495=DIRECTION('',(1.,0.,-1.15648231731787E-16));
#7496=DIRECTION('center_axis',(1.,0.,0.));
#7497=DIRECTION('ref_axis',(0.,-4.29586131949163E-10,-1.));
#7498=DIRECTION('center_axis',(1.,-1.20794999071527E-8,2.28224857621035E-17));
#7499=DIRECTION('ref_axis',(1.20794999071527E-8,1.,-1.89856639006012E-41));
#7500=DIRECTION('center_axis',(1.,1.20794999172425E-8,-1.59545740616835E-17));
#7501=DIRECTION('ref_axis',(1.20794999243885E-8,-1.,-8.2319592183107E-12));
#7502=DIRECTION('center_axis',(3.9010897446429E-10,-1.,-3.90108144056802E-10));
#7503=DIRECTION('ref_axis',(0.999999999999707,3.90109272919983E-10,-7.65059154471383E-7));
#7504=DIRECTION('center_axis',(3.90083837031876E-10,-1.,3.90119162425402E-10));
#7505=DIRECTION('ref_axis',(7.96162783282112E-7,3.90119472995512E-10,0.999999999999683));
#7506=DIRECTION('center_axis',(1.,-1.20794999071527E-8,2.28224857621035E-17));
#7507=DIRECTION('ref_axis',(1.20794999243885E-8,1.,0.));
#7508=DIRECTION('axis',(0.,0.,1.));
#7509=DIRECTION('refdir',(1.,0.,0.));
#7510=DIRECTION('center_axis',(1.,4.17203717831812E-9,1.01277540341552E-17));
#7511=DIRECTION('ref_axis',(-4.1720371751696E-9,1.,0.));
#7512=DIRECTION('center_axis',(1.,4.17203717831812E-9,1.01277540341552E-17));
#7513=DIRECTION('ref_axis',(-4.17203717831812E-9,1.,-1.69634196247466E-42));
#7514=DIRECTION('center_axis',(8.36866394062756E-10,1.,-8.36884415538179E-10));
#7515=DIRECTION('ref_axis',(-7.96162761077703E-7,8.36885081819775E-10,0.999999999999683));
#7516=DIRECTION('center_axis',(1.,4.17203717831812E-9,1.01277540341552E-17));
#7517=DIRECTION('ref_axis',(-4.17203717831812E-9,1.,-1.69634196247466E-42));
#7518=DIRECTION('center_axis',(8.36869948186391E-10,1.,8.36891441629708E-10));
#7519=DIRECTION('ref_axis',(-0.999999999999707,8.36870588457614E-10,-7.65059166582913E-7));
#7520=DIRECTION('center_axis',(1.,-4.17203708245403E-9,6.73890284431642E-18));
#7521=DIRECTION('ref_axis',(-4.1720370750894E-9,-1.,5.66553889764798E-16));
#7522=DIRECTION('center_axis',(1.,-4.17203708245403E-9,6.73890284431642E-18));
#7523=DIRECTION('ref_axis',(4.17203708245403E-9,1.,-1.23465054354127E-43));
#7524=DIRECTION('center_axis',(-1.,4.17203697154146E-9,4.27849718847752E-19));
#7525=DIRECTION('ref_axis',(-4.27008851558771E-17,-5.34839554841822E-9,
1.));
#7526=DIRECTION('center_axis',(1.,0.,-3.33600668457079E-17));
#7527=DIRECTION('ref_axis',(-3.33600668457079E-17,0.,-1.));
#7528=DIRECTION('center_axis',(1.,0.,-3.33600668457079E-17));
#7529=DIRECTION('ref_axis',(-3.33600668457079E-17,0.,-1.));
#7530=DIRECTION('center_axis',(1.,0.,0.));
#7531=DIRECTION('ref_axis',(0.,-4.64793894161955E-10,-1.));
#7532=DIRECTION('',(-1.,0.,3.33600668457079E-17));
#7533=DIRECTION('center_axis',(-1.,1.53144334479515E-17,1.9842828066192E-17));
#7534=DIRECTION('ref_axis',(1.9842828066192E-17,0.,1.));
#7535=DIRECTION('center_axis',(1.,0.,0.));
#7536=DIRECTION('ref_axis',(0.,0.,-1.));
#7537=DIRECTION('center_axis',(1.,-4.17203727418451E-9,-1.07069540457721E-17));
#7538=DIRECTION('ref_axis',(4.1720372752498E-9,1.,0.));
#7539=DIRECTION('center_axis',(-8.36866342496331E-10,1.,-8.36883936494317E-10));
#7540=DIRECTION('ref_axis',(0.999999999999707,8.36866982761818E-10,7.65059174657239E-7));
#7541=DIRECTION('center_axis',(1.,-4.17203727418451E-9,-1.07069540457721E-17));
#7542=DIRECTION('ref_axis',(4.17203727418451E-9,1.,1.45967462857766E-42));
#7543=DIRECTION('center_axis',(-8.36844869453255E-10,1.,8.36865935422119E-10));
#7544=DIRECTION('ref_axis',(9.00645352209864E-7,8.36866689122222E-10,-0.999999999999595));
#7545=DIRECTION('center_axis',(1.,0.,0.));
#7546=DIRECTION('ref_axis',(0.,0.,-1.));
#7547=DIRECTION('',(1.,0.,0.));
#7548=DIRECTION('center_axis',(1.,0.,0.));
#7549=DIRECTION('ref_axis',(0.,-4.29586394988857E-10,-1.));
#7550=DIRECTION('center_axis',(1.,0.,0.));
#7551=DIRECTION('ref_axis',(0.,-4.29586394988857E-10,-1.));
#7552=DIRECTION('center_axis',(1.,4.17203725971588E-9,2.0031116033889E-18));
#7553=DIRECTION('ref_axis',(4.1720372752498E-9,-1.,5.66553889764798E-16));
#7554=DIRECTION('center_axis',(1.,4.17203725971588E-9,2.0031116033889E-18));
#7555=DIRECTION('ref_axis',(-4.17203725971588E-9,1.,5.39459847610519E-43));
#7556=DIRECTION('center_axis',(1.,1.53144334479515E-17,-1.9842828066192E-17));
#7557=DIRECTION('ref_axis',(-1.9842828066192E-17,0.,-1.));
#7558=DIRECTION('center_axis',(1.,0.,0.));
#7559=DIRECTION('ref_axis',(0.,0.,-1.));
#7560=DIRECTION('center_axis',(1.,6.36556116938371E-17,1.00386354793954E-17));
#7561=DIRECTION('ref_axis',(-6.3655612933414E-17,1.,0.));
#7562=DIRECTION('center_axis',(1.00386354793954E-17,1.22464679914735E-16,
-1.));
#7563=DIRECTION('ref_axis',(6.36556105223495E-17,-1.,-1.22464679914735E-16));
#7564=DIRECTION('center_axis',(1.,1.35504238326755E-16,2.34999225611352E-17));
#7565=DIRECTION('ref_axis',(-1.35504238326755E-16,1.,1.40763492406121E-49));
#7566=DIRECTION('center_axis',(1.,1.35504238326755E-16,2.34999225611352E-17));
#7567=DIRECTION('ref_axis',(-1.35504238326755E-16,1.,1.40763492406121E-49));
#7568=DIRECTION('center_axis',(1.,0.,0.));
#7569=DIRECTION('ref_axis',(0.,0.,-1.));
#7570=DIRECTION('center_axis',(-1.,0.,0.));
#7571=DIRECTION('ref_axis',(0.,-6.60206605267583E-10,1.));
#7572=DIRECTION('center_axis',(-1.,0.,0.));
#7573=DIRECTION('ref_axis',(0.,-6.60206605267583E-10,1.));
#7574=DIRECTION('',(1.,0.,0.));
#7575=DIRECTION('center_axis',(1.,0.,0.));
#7576=DIRECTION('ref_axis',(0.,0.,-1.));
#7577=DIRECTION('',(-1.,0.,0.));
#7578=DIRECTION('center_axis',(1.,0.,0.));
#7579=DIRECTION('ref_axis',(0.,0.,-1.));
#7580=DIRECTION('center_axis',(1.,1.18552772674719E-16,-1.97711088800387E-17));
#7581=DIRECTION('ref_axis',(-1.18552772074394E-16,1.,0.));
#7582=DIRECTION('center_axis',(-1.,0.,0.));
#7583=DIRECTION('ref_axis',(0.,-2.05103586755523E-10,1.));
#7584=DIRECTION('center_axis',(-1.97711088800387E-17,1.22464679914735E-16,
-1.));
#7585=DIRECTION('ref_axis',(1.18552771796194E-16,-1.,-1.22464679914735E-16));
#7586=DIRECTION('center_axis',(-1.,0.,0.));
#7587=DIRECTION('ref_axis',(0.,-2.05103586755523E-10,1.));
#7588=DIRECTION('center_axis',(-1.,2.92206431305708E-17,3.78610282642285E-17));
#7589=DIRECTION('ref_axis',(3.78610282642285E-17,0.,1.));
#7590=DIRECTION('center_axis',(1.,1.20795004338275E-8,6.525328094131E-17));
#7591=DIRECTION('ref_axis',(-1.20795004338275E-8,1.,4.44135209129409E-41));
#7592=DIRECTION('center_axis',(1.,-1.20794999078492E-8,-6.65136044666218E-17));
#7593=DIRECTION('ref_axis',(1.20794999078492E-8,1.,-3.20659696454606E-41));
#7594=DIRECTION('center_axis',(1.,0.,0.));
#7595=DIRECTION('ref_axis',(0.,0.,-1.));
#7596=DIRECTION('center_axis',(1.,0.,0.));
#7597=DIRECTION('ref_axis',(0.,0.,-1.));
#7598=DIRECTION('',(-1.,0.,0.));
#7599=DIRECTION('center_axis',(1.,-1.20794999078492E-8,-6.65136044666218E-17));
#7600=DIRECTION('ref_axis',(-1.20794999243885E-8,-1.,-5.21792575105832E-12));
#7601=DIRECTION('center_axis',(-3.90112644891662E-10,-1.,-3.90117034748036E-10));
#7602=DIRECTION('ref_axis',(-7.96162782272821E-7,3.90117345341081E-10,-0.999999999999683));
#7603=DIRECTION('center_axis',(1.,-1.20794992145421E-8,-4.8381018443521E-19));
#7604=DIRECTION('ref_axis',(1.48029741503464E-16,1.78300800621899E-8,-1.));
#7605=DIRECTION('center_axis',(-3.90083830404282E-10,-1.,3.90119162273478E-10));
#7606=DIRECTION('ref_axis',(-0.999999999999707,3.90084128868405E-10,7.65059156489968E-7));
#7607=DIRECTION('center_axis',(1.,1.20795004338275E-8,6.525328094131E-17));
#7608=DIRECTION('ref_axis',(-1.20795004609008E-8,1.,0.));
#7609=DIRECTION('center_axis',(1.,1.20795004338275E-8,6.525328094131E-17));
#7610=DIRECTION('ref_axis',(-1.20795004338275E-8,1.,4.44135209129409E-41));
#7611=DIRECTION('center_axis',(1.,2.92206431305708E-17,-3.78610282642285E-17));
#7612=DIRECTION('ref_axis',(-3.78610282642285E-17,0.,-1.));
#7613=DIRECTION('center_axis',(1.,-1.20794999071527E-8,2.28224857621035E-17));
#7614=DIRECTION('ref_axis',(1.20794999071527E-8,1.,-1.89856639006012E-41));
#7615=DIRECTION('center_axis',(1.,1.20794999172425E-8,-1.59545740616835E-17));
#7616=DIRECTION('ref_axis',(-1.20794999172425E-8,1.,2.99570552288603E-42));
#7617=DIRECTION('center_axis',(1.,0.,-1.15648231731787E-16));
#7618=DIRECTION('ref_axis',(-1.15648231731787E-16,0.,-1.));
#7619=DIRECTION('',(1.,0.,-1.15648231731787E-16));
#7620=DIRECTION('center_axis',(1.,0.,0.));
#7621=DIRECTION('ref_axis',(0.,-4.29586131949163E-10,-1.));
#7622=DIRECTION('center_axis',(1.,-1.20794999071527E-8,2.28224857621035E-17));
#7623=DIRECTION('ref_axis',(1.20794999071527E-8,1.,-1.89856639006012E-41));
#7624=DIRECTION('center_axis',(1.,1.20794999172425E-8,-1.59545740616835E-17));
#7625=DIRECTION('ref_axis',(1.20794999243885E-8,-1.,-8.2319592183107E-12));
#7626=DIRECTION('center_axis',(3.9010897446429E-10,-1.,-3.90108144056802E-10));
#7627=DIRECTION('ref_axis',(0.999999999999707,3.90109272919983E-10,-7.65059154471383E-7));
#7628=DIRECTION('center_axis',(3.90083837031876E-10,-1.,3.90119162425402E-10));
#7629=DIRECTION('ref_axis',(7.96162783282112E-7,3.90119472995512E-10,0.999999999999683));
#7630=DIRECTION('center_axis',(1.,-1.20794999071527E-8,2.28224857621035E-17));
#7631=DIRECTION('ref_axis',(1.20794999243885E-8,1.,0.));
#7632=DIRECTION('axis',(0.,0.,1.));
#7633=DIRECTION('refdir',(1.,0.,0.));
#7634=DIRECTION('center_axis',(4.13029399042097E-17,0.,1.));
#7635=DIRECTION('ref_axis',(1.,0.,-4.13029399042097E-17));
#7636=DIRECTION('center_axis',(-3.04809470411818E-27,2.64338815530979E-17,
1.));
#7637=DIRECTION('ref_axis',(1.,-4.29586510583046E-10,0.));
#7638=DIRECTION('',(-4.13029399042097E-17,0.,-1.));
#7639=DIRECTION('center_axis',(-5.28677630773884E-17,-1.0843360466812E-26,
-1.));
#7640=DIRECTION('ref_axis',(1.,2.50000086925735E-10,-5.28677630773884E-17));
#7641=DIRECTION('center_axis',(-5.28677630773884E-17,-1.0843360466812E-26,
-1.));
#7642=DIRECTION('ref_axis',(1.,2.50000086925735E-10,-5.28677630773884E-17));
#7643=DIRECTION('center_axis',(-1.70140119462979E-16,0.,-1.));
#7644=DIRECTION('ref_axis',(-1.,0.,1.70140119462979E-16));
#7645=DIRECTION('center_axis',(-9.76996261870523E-16,-9.7699626151362E-16,
-1.));
#7646=DIRECTION('ref_axis',(1.,-1.60206417040051E-10,-9.76996261670138E-16));
#7647=DIRECTION('',(-0.86602541098055,1.0605752475376E-16,0.49999998753597));
#7648=DIRECTION('center_axis',(1.70140119462979E-16,0.,1.));
#7649=DIRECTION('ref_axis',(1.,0.,-1.70140119462979E-16));
#7650=DIRECTION('center_axis',(0.,0.,1.));
#7651=DIRECTION('ref_axis',(-1.,-1.60206710118277E-10,0.));
#7652=DIRECTION('',(0.86602541098055,1.0605752475376E-16,-0.49999998753597));
#7653=DIRECTION('center_axis',(0.,0.,1.));
#7654=DIRECTION('ref_axis',(-1.,-1.60206710118277E-10,0.));
#7655=DIRECTION('center_axis',(0.,0.,-1.));
#7656=DIRECTION('ref_axis',(-1.,0.,0.));
#7657=DIRECTION('center_axis',(0.,0.,-1.));
#7658=DIRECTION('ref_axis',(-1.,0.,0.));
#7659=DIRECTION('',(0.,0.,1.));
#7660=DIRECTION('center_axis',(0.,0.,-1.));
#7661=DIRECTION('ref_axis',(-1.,0.,0.));
#7662=DIRECTION('',(0.,0.,1.));
#7663=DIRECTION('center_axis',(0.,0.,-1.));
#7664=DIRECTION('ref_axis',(-1.,0.,0.));
#7665=DIRECTION('center_axis',(2.84990285479818E-18,3.64291930135101E-18,
1.));
#7666=DIRECTION('ref_axis',(0.,-1.,3.64291930135101E-18));
#7667=DIRECTION('center_axis',(-2.16840434497101E-17,0.,-1.));
#7668=DIRECTION('ref_axis',(-1.,0.,2.16840434497101E-17));
#7669=DIRECTION('center_axis',(-2.84990285479818E-18,-3.64291930135101E-18,
1.));
#7670=DIRECTION('ref_axis',(0.,-1.,-3.64291930135101E-18));
#7671=DIRECTION('center_axis',(0.,0.,-1.));
#7672=DIRECTION('ref_axis',(-1.,0.,0.));
#7673=DIRECTION('center_axis',(-2.16840434497101E-17,0.,-1.));
#7674=DIRECTION('ref_axis',(-1.,0.,2.16840434497101E-17));
#7675=DIRECTION('center_axis',(-2.16840434497101E-17,0.,-1.));
#7676=DIRECTION('ref_axis',(-1.,0.,2.16840434497101E-17));
#7677=DIRECTION('',(-2.16840434497101E-17,0.,-1.));
#7678=DIRECTION('center_axis',(0.,0.,-1.));
#7679=DIRECTION('ref_axis',(-1.,0.,0.));
#7680=DIRECTION('',(0.,0.,-1.));
#7681=DIRECTION('center_axis',(0.,0.,-1.));
#7682=DIRECTION('ref_axis',(-1.,0.,0.));
#7683=DIRECTION('center_axis',(-6.27288400105048E-18,-2.92734586715581E-18,
1.));
#7684=DIRECTION('ref_axis',(1.,-1.25733582200228E-51,6.27288400105048E-18));
#7685=DIRECTION('center_axis',(-3.46944695195361E-16,0.,1.));
#7686=DIRECTION('ref_axis',(1.,0.,3.46944695195361E-16));
#7687=DIRECTION('center_axis',(-3.46944695195361E-16,0.,1.));
#7688=DIRECTION('ref_axis',(1.,0.,3.46944695195361E-16));
#7689=DIRECTION('center_axis',(-3.46944695195362E-16,0.,1.));
#7690=DIRECTION('ref_axis',(1.,0.,3.46944695195362E-16));
#7691=DIRECTION('center_axis',(-3.46944695195361E-16,0.,1.));
#7692=DIRECTION('ref_axis',(1.,0.,3.46944695195361E-16));
#7693=DIRECTION('center_axis',(-3.46944695195361E-16,0.,1.));
#7694=DIRECTION('ref_axis',(1.,0.,3.46944695195361E-16));
#7695=DIRECTION('center_axis',(-3.46944695195362E-16,0.,1.));
#7696=DIRECTION('ref_axis',(1.,0.,3.46944695195362E-16));
#7697=DIRECTION('center_axis',(0.,0.,-1.));
#7698=DIRECTION('ref_axis',(-1.,0.,0.));
#7699=DIRECTION('center_axis',(6.27288400105048E-18,2.92734586715581E-18,
1.));
#7700=DIRECTION('ref_axis',(1.,-1.25733582200228E-51,-6.27288400105048E-18));
#7701=DIRECTION('center_axis',(-3.46944695195361E-16,0.,1.));
#7702=DIRECTION('ref_axis',(1.,0.,3.46944695195361E-16));
#7703=DIRECTION('center_axis',(-3.46944695195361E-16,0.,1.));
#7704=DIRECTION('ref_axis',(1.,0.,3.46944695195361E-16));
#7705=DIRECTION('center_axis',(-3.46944695195362E-16,0.,1.));
#7706=DIRECTION('ref_axis',(1.,0.,3.46944695195362E-16));
#7707=DIRECTION('center_axis',(-3.46944695195361E-16,0.,1.));
#7708=DIRECTION('ref_axis',(1.,0.,3.46944695195361E-16));
#7709=DIRECTION('center_axis',(-3.46944695195361E-16,0.,1.));
#7710=DIRECTION('ref_axis',(1.,0.,3.46944695195361E-16));
#7711=DIRECTION('center_axis',(-3.46944695195362E-16,0.,1.));
#7712=DIRECTION('ref_axis',(1.,0.,3.46944695195362E-16));
#7713=DIRECTION('center_axis',(0.,0.,-1.));
#7714=DIRECTION('ref_axis',(-1.,0.,0.));
#7715=DIRECTION('center_axis',(0.,0.,-1.));
#7716=DIRECTION('ref_axis',(-1.,0.,0.));
#7717=DIRECTION('center_axis',(0.,0.,-1.));
#7718=DIRECTION('ref_axis',(-1.,0.,0.));
#7719=DIRECTION('',(0.,0.,1.));
#7720=DIRECTION('center_axis',(-3.46944695195362E-16,0.,1.));
#7721=DIRECTION('ref_axis',(1.,0.,3.46944695195362E-16));
#7722=DIRECTION('',(-3.46944695195362E-16,0.,1.));
#7723=DIRECTION('center_axis',(-3.46944695195361E-16,0.,1.));
#7724=DIRECTION('ref_axis',(1.,0.,3.46944695195361E-16));
#7725=DIRECTION('',(-3.46944695195361E-16,0.,1.));
#7726=DIRECTION('center_axis',(-3.46944695195361E-16,0.,1.));
#7727=DIRECTION('ref_axis',(1.,0.,3.46944695195361E-16));
#7728=DIRECTION('',(-3.46944695195361E-16,0.,1.));
#7729=DIRECTION('center_axis',(-3.46944695195362E-16,0.,1.));
#7730=DIRECTION('ref_axis',(1.,0.,3.46944695195362E-16));
#7731=DIRECTION('',(-3.46944695195362E-16,0.,1.));
#7732=DIRECTION('center_axis',(-3.46944695195361E-16,0.,1.));
#7733=DIRECTION('ref_axis',(1.,0.,3.46944695195361E-16));
#7734=DIRECTION('',(-3.46944695195361E-16,0.,1.));
#7735=DIRECTION('center_axis',(-3.46944695195361E-16,0.,1.));
#7736=DIRECTION('ref_axis',(1.,0.,3.46944695195361E-16));
#7737=DIRECTION('',(-3.46944695195361E-16,0.,1.));
#7738=DIRECTION('center_axis',(0.,0.,-1.));
#7739=DIRECTION('ref_axis',(-1.,0.,0.));
#7740=DIRECTION('',(0.,0.,1.));
#7741=DIRECTION('center_axis',(0.,0.,-1.));
#7742=DIRECTION('ref_axis',(-1.,0.,0.));
#7743=DIRECTION('center_axis',(-6.39458016332861E-18,-1.10411609048463E-17,
1.));
#7744=DIRECTION('ref_axis',(0.,-1.,-1.10411609048463E-17));
#7745=DIRECTION('center_axis',(0.,0.,-1.));
#7746=DIRECTION('ref_axis',(-1.,0.,0.));
#7747=DIRECTION('center_axis',(6.39458016332861E-18,1.10411609048463E-17,
1.));
#7748=DIRECTION('ref_axis',(0.,-1.,1.10411609048463E-17));
#7749=DIRECTION('center_axis',(0.,0.,-1.));
#7750=DIRECTION('ref_axis',(-1.,0.,0.));
#7751=DIRECTION('center_axis',(0.,0.,-1.));
#7752=DIRECTION('ref_axis',(-1.,0.,0.));
#7753=DIRECTION('',(0.,0.,-1.));
#7754=DIRECTION('axis',(0.,0.,1.));
#7755=DIRECTION('refdir',(1.,0.,0.));
#7756=DIRECTION('center_axis',(0.,0.,1.));
#7757=DIRECTION('ref_axis',(1.,0.,0.));
#7758=DIRECTION('center_axis',(0.,0.,-1.));
#7759=DIRECTION('ref_axis',(1.,2.500007018071E-10,0.));
#7760=DIRECTION('',(0.,0.,1.));
#7761=DIRECTION('center_axis',(-2.35325480076137E-17,4.40779226798152E-17,
1.));
#7762=DIRECTION('ref_axis',(1.,-4.29586600835191E-10,2.64338815386942E-17));
#7763=DIRECTION('',(0.,0.,-1.));
#7764=DIRECTION('center_axis',(0.556379847069157,0.830928074971175,-7.35361873603602E-16));
#7765=DIRECTION('ref_axis',(-0.830928074971175,0.556379847069157,7.16694797445736E-33));
#7766=DIRECTION('',(0.830928075153644,-0.556379846796646,-5.68042456784337E-10));
#7767=DIRECTION('',(0.,0.,1.));
#7768=DIRECTION('',(-0.830928075153644,0.556379846796646,-5.6804240310886E-10));
#7769=DIRECTION('center_axis',(0.,0.,1.));
#7770=DIRECTION('ref_axis',(1.,0.,0.));
#7771=DIRECTION('',(-0.481839085130227,-0.719604828016666,0.499999987535971));
#7772=DIRECTION('center_axis',(0.,0.,1.));
#7773=DIRECTION('ref_axis',(1.,-4.29586566999823E-10,0.));
#7774=DIRECTION('',(-0.481839085425413,-0.719604827819009,-0.499999987535975));
#7775=DIRECTION('center_axis',(0.,0.,-1.));
#7776=DIRECTION('ref_axis',(0.830928075019912,-0.556379846996369,0.));
#7777=DIRECTION('center_axis',(-3.95346806367293E-17,7.40509100908303E-17,
-1.));
#7778=DIRECTION('ref_axis',(-0.556379846372783,-0.830928075437459,-4.44089209850062E-17));
#7779=DIRECTION('',(0.481839085296186,0.719604827905541,0.499999987535972));
#7780=DIRECTION('',(0.481839085720606,0.719604827621357,-0.499999987535967));
#7781=DIRECTION('center_axis',(0.278189923027056,0.41546403790653,-0.866025403745526));
#7782=DIRECTION('ref_axis',(-1.21325454929337E-16,0.901615702162283,0.432538004820864));
#7783=DIRECTION('',(0.8309280753204,-0.556379846547604,-3.68626283987023E-10));
#7784=DIRECTION('',(0.481839111062359,0.719604801945691,0.500000000067339));
#7785=DIRECTION('center_axis',(0.,0.,1.));
#7786=DIRECTION('ref_axis',(-0.830928076007245,0.556379845521832,0.));
#7787=DIRECTION('',(0.,0.,-1.));
#7788=DIRECTION('center_axis',(1.97868596828159E-16,1.05639103603771E-16,
-1.));
#7789=DIRECTION('ref_axis',(-1.,-4.10213239038492E-10,-1.8503717077086E-16));
#7790=DIRECTION('center_axis',(0.,0.,1.));
#7791=DIRECTION('ref_axis',(-0.556379848848799,-0.830928073779547,0.));
#7792=DIRECTION('center_axis',(0.278189923027056,0.41546403790653,0.866025403745527));
#7793=DIRECTION('ref_axis',(7.03710115468502E-19,-0.901615702162283,0.432538004820864));
#7794=DIRECTION('',(-0.8309280753204,0.556379846547604,-3.68626057553233E-10));
#7795=DIRECTION('',(-0.481839111062391,-0.719604801945631,0.500000000067394));
#7796=DIRECTION('center_axis',(0.,0.,1.));
#7797=DIRECTION('ref_axis',(1.,0.,0.));
#7798=DIRECTION('',(0.,0.,1.));
#7799=DIRECTION('',(0.,0.,-1.));
#7800=DIRECTION('center_axis',(-0.556379846547605,-0.8309280753204,1.01878114391287E-15));
#7801=DIRECTION('ref_axis',(0.8309280753204,-0.556379846547605,8.47369377023234E-32));
#7802=DIRECTION('',(-0.830928075329978,0.5563798465333,-2.98215105322737E-11));
#7803=DIRECTION('',(0.830928075329979,-0.556379846533299,-2.98209335407452E-11));
#7804=DIRECTION('center_axis',(-0.278189923198529,-0.415464037609672,0.866025403832859));
#7805=DIRECTION('ref_axis',(-8.10651120153385E-17,-0.90161570229982,-0.43253800453417));
#7806=DIRECTION('',(0.830928074971174,-0.556379847069157,-3.67583016147327E-10));
#7807=DIRECTION('',(-0.481839110724413,-0.719604802277015,-0.499999999916165));
#7808=DIRECTION('center_axis',(-0.556379846547604,-0.8309280753204,-1.1124685724156E-15));
#7809=DIRECTION('ref_axis',(0.8309280753204,-0.556379846547604,-7.86302266460809E-32));
#7810=DIRECTION('',(0.,0.,-1.));
#7811=DIRECTION('center_axis',(0.,0.,1.));
#7812=DIRECTION('ref_axis',(-0.830928074495347,0.556379847779784,0.));
#7813=DIRECTION('center_axis',(0.,0.,1.));
#7814=DIRECTION('ref_axis',(-0.556379846596556,-0.830928075287622,0.));
#7815=DIRECTION('',(0.481839085129936,0.7196048280168,-0.499999987536058));
#7816=DIRECTION('center_axis',(0.,0.,-1.));
#7817=DIRECTION('ref_axis',(-1.,0.,0.));
#7818=DIRECTION('center_axis',(-1.88631312013914E-13,-1.0754841012286E-13,
-1.));
#7819=DIRECTION('ref_axis',(-1.,-4.29767510467514E-10,1.88649096344057E-13));
#7820=DIRECTION('center_axis',(-0.278189923198529,-0.415464037609672,-0.866025403832859));
#7821=DIRECTION('ref_axis',(8.10651120153385E-17,0.90161570229982,-0.43253800453417));
#7822=DIRECTION('',(-0.830928074971174,0.556379847069157,-3.67583167123921E-10));
#7823=DIRECTION('center_axis',(0.556379847069157,0.830928074971175,2.1611143699565E-16));
#7824=DIRECTION('ref_axis',(-0.830928074971175,0.556379847069157,8.67438128407877E-33));
#7825=DIRECTION('',(0.,0.,1.));
#7826=DIRECTION('center_axis',(0.,0.,1.));
#7827=DIRECTION('ref_axis',(-0.830928075876665,0.556379845716848,0.));
#7828=DIRECTION('axis',(0.,0.,1.));
#7829=DIRECTION('refdir',(1.,0.,0.));
#7830=DIRECTION('center_axis',(-1.,0.,0.));
#7831=DIRECTION('ref_axis',(0.,0.,1.));
#7832=DIRECTION('center_axis',(-1.,0.,0.));
#7833=DIRECTION('ref_axis',(0.,0.,1.));
#7834=DIRECTION('',(-1.,0.,0.));
#7835=DIRECTION('center_axis',(-1.,0.,0.));
#7836=DIRECTION('ref_axis',(0.,0.,1.));
#7837=DIRECTION('center_axis',(1.,0.,0.));
#7838=DIRECTION('ref_axis',(0.,0.,-1.));
#7839=DIRECTION('',(0.,-1.,0.));
#7840=DIRECTION('',(0.,0.,1.));
#7841=DIRECTION('',(0.,1.,0.));
#7842=DIRECTION('',(0.,0.,-1.));
#7843=DIRECTION('center_axis',(-1.,0.,0.));
#7844=DIRECTION('ref_axis',(0.,0.,1.));
#7845=DIRECTION('center_axis',(-1.,0.,0.));
#7846=DIRECTION('ref_axis',(0.,0.,1.));
#7847=DIRECTION('center_axis',(-1.,0.,0.));
#7848=DIRECTION('ref_axis',(0.,0.,1.));
#7849=DIRECTION('center_axis',(-1.,0.,0.));
#7850=DIRECTION('ref_axis',(0.,0.,1.));
#7851=DIRECTION('center_axis',(1.,0.,0.));
#7852=DIRECTION('ref_axis',(0.,0.,-1.));
#7853=DIRECTION('',(0.,0.,1.));
#7854=DIRECTION('',(0.,-1.,0.));
#7855=DIRECTION('',(0.,0.,-1.));
#7856=DIRECTION('',(0.,1.,0.));
#7857=DIRECTION('center_axis',(-1.,0.,0.));
#7858=DIRECTION('ref_axis',(0.,0.,1.));
#7859=DIRECTION('center_axis',(-1.,0.,0.));
#7860=DIRECTION('ref_axis',(0.,0.,1.));
#7861=DIRECTION('center_axis',(-1.,0.,0.));
#7862=DIRECTION('ref_axis',(0.,0.,1.));
#7863=DIRECTION('center_axis',(-1.,0.,0.));
#7864=DIRECTION('ref_axis',(0.,0.,1.));
#7865=DIRECTION('center_axis',(-1.,0.,0.));
#7866=DIRECTION('ref_axis',(0.,0.,1.));
#7867=DIRECTION('',(-1.,0.,0.));
#7868=DIRECTION('center_axis',(-1.,0.,0.));
#7869=DIRECTION('ref_axis',(0.,0.,1.));
#7870=DIRECTION('',(-1.,0.,0.));
#7871=DIRECTION('center_axis',(-1.,0.,0.));
#7872=DIRECTION('ref_axis',(0.,0.,1.));
#7873=DIRECTION('',(-1.,0.,0.));
#7874=DIRECTION('center_axis',(-1.,0.,0.));
#7875=DIRECTION('ref_axis',(0.,0.,1.));
#7876=DIRECTION('',(-1.,0.,0.));
#7877=DIRECTION('center_axis',(0.,-1.,0.));
#7878=DIRECTION('ref_axis',(0.,0.,-1.));
#7879=DIRECTION('',(1.,0.,0.));
#7880=DIRECTION('',(-1.,0.,0.));
#7881=DIRECTION('center_axis',(1.43238595632038E-16,8.66263247203385E-18,
-1.));
#7882=DIRECTION('ref_axis',(-1.,7.27189582693585E-50,-1.43238595632038E-16));
#7883=DIRECTION('',(-1.,0.,0.));
#7884=DIRECTION('center_axis',(-1.18952466411614E-17,-1.,-2.57730345002263E-17));
#7885=DIRECTION('ref_axis',(-1.39638038884726E-50,2.57730345002263E-17,
-1.));
#7886=DIRECTION('',(-1.,0.,0.));
#7887=DIRECTION('center_axis',(-1.43238595632038E-16,-8.66263247203385E-18,
-1.));
#7888=DIRECTION('ref_axis',(-1.,7.27189582693585E-50,1.43238595632038E-16));
#7889=DIRECTION('axis',(0.,0.,1.));
#7890=DIRECTION('refdir',(1.,0.,0.));
#7891=DIRECTION('center_axis',(1.,4.17203717831812E-9,1.01277540341552E-17));
#7892=DIRECTION('ref_axis',(-4.1720371751696E-9,1.,0.));
#7893=DIRECTION('center_axis',(1.,4.17203717831812E-9,1.01277540341552E-17));
#7894=DIRECTION('ref_axis',(-4.17203717831812E-9,1.,-1.69634196247466E-42));
#7895=DIRECTION('center_axis',(8.36866394062756E-10,1.,-8.36884415538179E-10));
#7896=DIRECTION('ref_axis',(-7.96162761077703E-7,8.36885081819775E-10,0.999999999999683));
#7897=DIRECTION('center_axis',(1.,4.17203717831812E-9,1.01277540341552E-17));
#7898=DIRECTION('ref_axis',(-4.17203717831812E-9,1.,-1.69634196247466E-42));
#7899=DIRECTION('center_axis',(8.36869948186391E-10,1.,8.36891441629708E-10));
#7900=DIRECTION('ref_axis',(-0.999999999999707,8.36870588457614E-10,-7.65059166582913E-7));
#7901=DIRECTION('center_axis',(1.,-4.17203708245403E-9,6.73890284431642E-18));
#7902=DIRECTION('ref_axis',(-4.1720370750894E-9,-1.,5.66553889764798E-16));
#7903=DIRECTION('center_axis',(1.,-4.17203708245403E-9,6.73890284431642E-18));
#7904=DIRECTION('ref_axis',(4.17203708245403E-9,1.,-1.23465054354127E-43));
#7905=DIRECTION('center_axis',(-1.,4.17203697154146E-9,4.27849718847752E-19));
#7906=DIRECTION('ref_axis',(-4.27008851558771E-17,-5.34839554841822E-9,
1.));
#7907=DIRECTION('center_axis',(1.,0.,-3.33600668457079E-17));
#7908=DIRECTION('ref_axis',(-3.33600668457079E-17,0.,-1.));
#7909=DIRECTION('center_axis',(1.,0.,-3.33600668457079E-17));
#7910=DIRECTION('ref_axis',(-3.33600668457079E-17,0.,-1.));
#7911=DIRECTION('center_axis',(1.,0.,0.));
#7912=DIRECTION('ref_axis',(0.,-4.64793894161955E-10,-1.));
#7913=DIRECTION('',(-1.,0.,3.33600668457079E-17));
#7914=DIRECTION('center_axis',(-1.,1.53144334479515E-17,1.9842828066192E-17));
#7915=DIRECTION('ref_axis',(1.9842828066192E-17,0.,1.));
#7916=DIRECTION('center_axis',(1.,0.,0.));
#7917=DIRECTION('ref_axis',(0.,0.,-1.));
#7918=DIRECTION('center_axis',(1.,-4.17203727418451E-9,-1.07069540457721E-17));
#7919=DIRECTION('ref_axis',(4.1720372752498E-9,1.,0.));
#7920=DIRECTION('center_axis',(-8.36866342496331E-10,1.,-8.36883936494317E-10));
#7921=DIRECTION('ref_axis',(0.999999999999707,8.36866982761818E-10,7.65059174657239E-7));
#7922=DIRECTION('center_axis',(1.,-4.17203727418451E-9,-1.07069540457721E-17));
#7923=DIRECTION('ref_axis',(4.17203727418451E-9,1.,1.45967462857766E-42));
#7924=DIRECTION('center_axis',(-8.36844869453255E-10,1.,8.36865935422119E-10));
#7925=DIRECTION('ref_axis',(9.00645352209864E-7,8.36866689122222E-10,-0.999999999999595));
#7926=DIRECTION('center_axis',(1.,0.,0.));
#7927=DIRECTION('ref_axis',(0.,0.,-1.));
#7928=DIRECTION('',(1.,0.,0.));
#7929=DIRECTION('center_axis',(1.,0.,0.));
#7930=DIRECTION('ref_axis',(0.,-4.29586394988857E-10,-1.));
#7931=DIRECTION('center_axis',(1.,0.,0.));
#7932=DIRECTION('ref_axis',(0.,-4.29586394988857E-10,-1.));
#7933=DIRECTION('center_axis',(1.,4.17203725971588E-9,2.0031116033889E-18));
#7934=DIRECTION('ref_axis',(4.1720372752498E-9,-1.,5.66553889764798E-16));
#7935=DIRECTION('center_axis',(1.,4.17203725971588E-9,2.0031116033889E-18));
#7936=DIRECTION('ref_axis',(-4.17203725971588E-9,1.,5.39459847610519E-43));
#7937=DIRECTION('center_axis',(1.,1.53144334479515E-17,-1.9842828066192E-17));
#7938=DIRECTION('ref_axis',(-1.9842828066192E-17,0.,-1.));
#7939=DIRECTION('center_axis',(1.,0.,0.));
#7940=DIRECTION('ref_axis',(0.,0.,-1.));
#7941=DIRECTION('center_axis',(1.,6.36556116938371E-17,1.00386354793954E-17));
#7942=DIRECTION('ref_axis',(-6.3655612933414E-17,1.,0.));
#7943=DIRECTION('center_axis',(1.00386354793954E-17,1.22464679914735E-16,
-1.));
#7944=DIRECTION('ref_axis',(6.36556105223495E-17,-1.,-1.22464679914735E-16));
#7945=DIRECTION('center_axis',(1.,1.35504238326755E-16,2.34999225611352E-17));
#7946=DIRECTION('ref_axis',(-1.35504238326755E-16,1.,1.40763492406121E-49));
#7947=DIRECTION('center_axis',(1.,1.35504238326755E-16,2.34999225611352E-17));
#7948=DIRECTION('ref_axis',(-1.35504238326755E-16,1.,1.40763492406121E-49));
#7949=DIRECTION('center_axis',(1.,0.,0.));
#7950=DIRECTION('ref_axis',(0.,0.,-1.));
#7951=DIRECTION('center_axis',(-1.,0.,0.));
#7952=DIRECTION('ref_axis',(0.,-6.60206605267583E-10,1.));
#7953=DIRECTION('center_axis',(-1.,0.,0.));
#7954=DIRECTION('ref_axis',(0.,-6.60206605267583E-10,1.));
#7955=DIRECTION('',(1.,0.,0.));
#7956=DIRECTION('center_axis',(1.,0.,0.));
#7957=DIRECTION('ref_axis',(0.,0.,-1.));
#7958=DIRECTION('',(-1.,0.,0.));
#7959=DIRECTION('center_axis',(1.,0.,0.));
#7960=DIRECTION('ref_axis',(0.,0.,-1.));
#7961=DIRECTION('center_axis',(1.,1.18552772674719E-16,-1.97711088800387E-17));
#7962=DIRECTION('ref_axis',(-1.18552772074394E-16,1.,0.));
#7963=DIRECTION('center_axis',(-1.,0.,0.));
#7964=DIRECTION('ref_axis',(0.,-2.05103586755523E-10,1.));
#7965=DIRECTION('center_axis',(-1.97711088800387E-17,1.22464679914735E-16,
-1.));
#7966=DIRECTION('ref_axis',(1.18552771796194E-16,-1.,-1.22464679914735E-16));
#7967=DIRECTION('center_axis',(-1.,0.,0.));
#7968=DIRECTION('ref_axis',(0.,-2.05103586755523E-10,1.));
#7969=DIRECTION('center_axis',(-1.,2.92206431305708E-17,3.78610282642285E-17));
#7970=DIRECTION('ref_axis',(3.78610282642285E-17,0.,1.));
#7971=DIRECTION('center_axis',(1.,1.20795004338275E-8,6.525328094131E-17));
#7972=DIRECTION('ref_axis',(-1.20795004338275E-8,1.,4.44135209129409E-41));
#7973=DIRECTION('center_axis',(1.,-1.20794999078492E-8,-6.65136044666218E-17));
#7974=DIRECTION('ref_axis',(1.20794999078492E-8,1.,-3.20659696454606E-41));
#7975=DIRECTION('center_axis',(1.,0.,0.));
#7976=DIRECTION('ref_axis',(0.,0.,-1.));
#7977=DIRECTION('center_axis',(1.,0.,0.));
#7978=DIRECTION('ref_axis',(0.,0.,-1.));
#7979=DIRECTION('',(-1.,0.,0.));
#7980=DIRECTION('center_axis',(1.,-1.20794999078492E-8,-6.65136044666218E-17));
#7981=DIRECTION('ref_axis',(-1.20794999243885E-8,-1.,-5.21792575105832E-12));
#7982=DIRECTION('center_axis',(-3.90112644891662E-10,-1.,-3.90117034748036E-10));
#7983=DIRECTION('ref_axis',(-7.96162782272821E-7,3.90117345341081E-10,-0.999999999999683));
#7984=DIRECTION('center_axis',(1.,-1.20794992145421E-8,-4.8381018443521E-19));
#7985=DIRECTION('ref_axis',(1.48029741503464E-16,1.78300800621899E-8,-1.));
#7986=DIRECTION('center_axis',(-3.90083830404282E-10,-1.,3.90119162273478E-10));
#7987=DIRECTION('ref_axis',(-0.999999999999707,3.90084128868405E-10,7.65059156489968E-7));
#7988=DIRECTION('center_axis',(1.,1.20795004338275E-8,6.525328094131E-17));
#7989=DIRECTION('ref_axis',(-1.20795004609008E-8,1.,0.));
#7990=DIRECTION('center_axis',(1.,1.20795004338275E-8,6.525328094131E-17));
#7991=DIRECTION('ref_axis',(-1.20795004338275E-8,1.,4.44135209129409E-41));
#7992=DIRECTION('center_axis',(1.,2.92206431305708E-17,-3.78610282642285E-17));
#7993=DIRECTION('ref_axis',(-3.78610282642285E-17,0.,-1.));
#7994=DIRECTION('center_axis',(1.,-1.20794999071527E-8,2.28224857621035E-17));
#7995=DIRECTION('ref_axis',(1.20794999071527E-8,1.,-1.89856639006012E-41));
#7996=DIRECTION('center_axis',(1.,1.20794999172425E-8,-1.59545740616835E-17));
#7997=DIRECTION('ref_axis',(-1.20794999172425E-8,1.,2.99570552288603E-42));
#7998=DIRECTION('center_axis',(1.,0.,-1.15648231731787E-16));
#7999=DIRECTION('ref_axis',(-1.15648231731787E-16,0.,-1.));
#8000=DIRECTION('',(1.,0.,-1.15648231731787E-16));
#8001=DIRECTION('center_axis',(1.,0.,0.));
#8002=DIRECTION('ref_axis',(0.,-4.29586131949163E-10,-1.));
#8003=DIRECTION('center_axis',(1.,-1.20794999071527E-8,2.28224857621035E-17));
#8004=DIRECTION('ref_axis',(1.20794999071527E-8,1.,-1.89856639006012E-41));
#8005=DIRECTION('center_axis',(1.,1.20794999172425E-8,-1.59545740616835E-17));
#8006=DIRECTION('ref_axis',(1.20794999243885E-8,-1.,-8.2319592183107E-12));
#8007=DIRECTION('center_axis',(3.9010897446429E-10,-1.,-3.90108144056802E-10));
#8008=DIRECTION('ref_axis',(0.999999999999707,3.90109272919983E-10,-7.65059154471383E-7));
#8009=DIRECTION('center_axis',(3.90083837031876E-10,-1.,3.90119162425402E-10));
#8010=DIRECTION('ref_axis',(7.96162783282112E-7,3.90119472995512E-10,0.999999999999683));
#8011=DIRECTION('center_axis',(1.,-1.20794999071527E-8,2.28224857621035E-17));
#8012=DIRECTION('ref_axis',(1.20794999243885E-8,1.,0.));
#8013=DIRECTION('axis',(0.,0.,1.));
#8014=DIRECTION('refdir',(1.,0.,0.));
#8015=DIRECTION('center_axis',(-1.,0.,0.));
#8016=DIRECTION('ref_axis',(0.,0.,1.));
#8017=DIRECTION('center_axis',(-1.,0.,0.));
#8018=DIRECTION('ref_axis',(0.,0.,1.));
#8019=DIRECTION('',(1.,0.,0.));
#8020=DIRECTION('center_axis',(-1.,0.,0.));
#8021=DIRECTION('ref_axis',(0.,0.,1.));
#8022=DIRECTION('center_axis',(1.,9.92686658991245E-16,-1.01959257413342E-15));
#8023=DIRECTION('ref_axis',(-1.01959257413342E-15,0.,-1.));
#8024=DIRECTION('center_axis',(1.,0.,0.));
#8025=DIRECTION('ref_axis',(0.,0.,-1.));
#8026=DIRECTION('center_axis',(-1.,0.,0.));
#8027=DIRECTION('ref_axis',(0.,0.,1.));
#8028=DIRECTION('center_axis',(1.,0.,0.));
#8029=DIRECTION('ref_axis',(0.,0.,-1.));
#8030=DIRECTION('',(0.,1.,0.));
#8031=DIRECTION('',(0.,0.,1.));
#8032=DIRECTION('center_axis',(1.,0.,0.));
#8033=DIRECTION('ref_axis',(0.,0.,-1.));
#8034=DIRECTION('center_axis',(1.,0.,0.));
#8035=DIRECTION('ref_axis',(0.,0.,-1.));
#8036=DIRECTION('center_axis',(1.,0.,0.));
#8037=DIRECTION('ref_axis',(0.,0.,-1.));
#8038=DIRECTION('center_axis',(1.,0.,0.));
#8039=DIRECTION('ref_axis',(0.,0.,-1.));
#8040=DIRECTION('center_axis',(1.,0.,0.));
#8041=DIRECTION('ref_axis',(0.,0.,-1.));
#8042=DIRECTION('center_axis',(1.,0.,0.));
#8043=DIRECTION('ref_axis',(0.,0.,-1.));
#8044=DIRECTION('center_axis',(1.,0.,0.));
#8045=DIRECTION('ref_axis',(0.,0.,-1.));
#8046=DIRECTION('',(1.,0.,0.));
#8047=DIRECTION('center_axis',(1.,0.,0.));
#8048=DIRECTION('ref_axis',(0.,0.,-1.));
#8049=DIRECTION('center_axis',(1.,0.,0.));
#8050=DIRECTION('ref_axis',(0.,0.,-1.));
#8051=DIRECTION('',(1.,0.,0.));
#8052=DIRECTION('center_axis',(1.,0.,0.));
#8053=DIRECTION('ref_axis',(0.,0.,-1.));
#8054=DIRECTION('center_axis',(1.,0.,0.));
#8055=DIRECTION('ref_axis',(0.,0.,-1.));
#8056=DIRECTION('',(1.,0.,0.));
#8057=DIRECTION('center_axis',(1.,0.,0.));
#8058=DIRECTION('ref_axis',(0.,0.,-1.));
#8059=DIRECTION('center_axis',(1.,0.,0.));
#8060=DIRECTION('ref_axis',(0.,0.,-1.));
#8061=DIRECTION('',(1.,0.,0.));
#8062=DIRECTION('center_axis',(1.,0.,0.));
#8063=DIRECTION('ref_axis',(0.,0.,-1.));
#8064=DIRECTION('center_axis',(1.,0.,0.));
#8065=DIRECTION('ref_axis',(0.,0.,-1.));
#8066=DIRECTION('',(1.,0.,0.));
#8067=DIRECTION('center_axis',(2.20458572024499E-15,-5.64627709665657E-16,
-1.));
#8068=DIRECTION('ref_axis',(-1.,8.70448729829261E-47,-2.20458572024499E-15));
#8069=DIRECTION('',(-1.,0.,0.));
#8070=DIRECTION('',(1.,0.,0.));
#8071=DIRECTION('',(0.,1.,0.));
#8072=DIRECTION('center_axis',(-3.68752647699062E-16,-1.,1.69617406532146E-17));
#8073=DIRECTION('ref_axis',(1.,-3.68752647699062E-16,0.));
#8074=DIRECTION('',(0.,0.,-1.));
#8075=DIRECTION('',(1.,0.,0.));
#8076=DIRECTION('center_axis',(1.,0.,0.));
#8077=DIRECTION('ref_axis',(0.,0.,-1.));
#8078=DIRECTION('',(-1.,0.,0.));
#8079=DIRECTION('center_axis',(1.,0.,0.));
#8080=DIRECTION('ref_axis',(0.,0.,-1.));
#8081=DIRECTION('center_axis',(1.,0.,0.));
#8082=DIRECTION('ref_axis',(0.,0.,-1.));
#8083=DIRECTION('center_axis',(1.,0.,0.));
#8084=DIRECTION('ref_axis',(0.,0.,-1.));
#8085=DIRECTION('center_axis',(-1.,0.,0.));
#8086=DIRECTION('ref_axis',(0.,0.,1.));
#8087=DIRECTION('axis',(0.,0.,1.));
#8088=DIRECTION('refdir',(1.,0.,0.));
#8089=DIRECTION('center_axis',(1.,4.17203717831812E-9,1.01277540341552E-17));
#8090=DIRECTION('ref_axis',(-4.1720371751696E-9,1.,0.));
#8091=DIRECTION('center_axis',(1.,4.17203717831812E-9,1.01277540341552E-17));
#8092=DIRECTION('ref_axis',(-4.17203717831812E-9,1.,-1.69634196247466E-42));
#8093=DIRECTION('center_axis',(8.36866394062756E-10,1.,-8.36884415538179E-10));
#8094=DIRECTION('ref_axis',(-7.96162761077703E-7,8.36885081819775E-10,0.999999999999683));
#8095=DIRECTION('center_axis',(1.,4.17203717831812E-9,1.01277540341552E-17));
#8096=DIRECTION('ref_axis',(-4.17203717831812E-9,1.,-1.69634196247466E-42));
#8097=DIRECTION('center_axis',(8.36869948186391E-10,1.,8.36891441629708E-10));
#8098=DIRECTION('ref_axis',(-0.999999999999707,8.36870588457614E-10,-7.65059166582913E-7));
#8099=DIRECTION('center_axis',(1.,-4.17203708245403E-9,6.73890284431642E-18));
#8100=DIRECTION('ref_axis',(-4.1720370750894E-9,-1.,5.66553889764798E-16));
#8101=DIRECTION('center_axis',(1.,-4.17203708245403E-9,6.73890284431642E-18));
#8102=DIRECTION('ref_axis',(4.17203708245403E-9,1.,-1.23465054354127E-43));
#8103=DIRECTION('center_axis',(-1.,4.17203697154146E-9,4.27849718847752E-19));
#8104=DIRECTION('ref_axis',(-4.27008851558771E-17,-5.34839554841822E-9,
1.));
#8105=DIRECTION('center_axis',(1.,0.,-3.33600668457079E-17));
#8106=DIRECTION('ref_axis',(-3.33600668457079E-17,0.,-1.));
#8107=DIRECTION('center_axis',(1.,0.,-3.33600668457079E-17));
#8108=DIRECTION('ref_axis',(-3.33600668457079E-17,0.,-1.));
#8109=DIRECTION('center_axis',(1.,0.,0.));
#8110=DIRECTION('ref_axis',(0.,-4.64793894161955E-10,-1.));
#8111=DIRECTION('',(-1.,0.,3.33600668457079E-17));
#8112=DIRECTION('center_axis',(-1.,1.53144334479515E-17,1.9842828066192E-17));
#8113=DIRECTION('ref_axis',(1.9842828066192E-17,0.,1.));
#8114=DIRECTION('center_axis',(1.,0.,0.));
#8115=DIRECTION('ref_axis',(0.,0.,-1.));
#8116=DIRECTION('center_axis',(1.,-4.17203727418451E-9,-1.07069540457721E-17));
#8117=DIRECTION('ref_axis',(4.1720372752498E-9,1.,0.));
#8118=DIRECTION('center_axis',(-8.36866342496331E-10,1.,-8.36883936494317E-10));
#8119=DIRECTION('ref_axis',(0.999999999999707,8.36866982761818E-10,7.65059174657239E-7));
#8120=DIRECTION('center_axis',(1.,-4.17203727418451E-9,-1.07069540457721E-17));
#8121=DIRECTION('ref_axis',(4.17203727418451E-9,1.,1.45967462857766E-42));
#8122=DIRECTION('center_axis',(-8.36844869453255E-10,1.,8.36865935422119E-10));
#8123=DIRECTION('ref_axis',(9.00645352209864E-7,8.36866689122222E-10,-0.999999999999595));
#8124=DIRECTION('center_axis',(1.,0.,0.));
#8125=DIRECTION('ref_axis',(0.,0.,-1.));
#8126=DIRECTION('',(1.,0.,0.));
#8127=DIRECTION('center_axis',(1.,0.,0.));
#8128=DIRECTION('ref_axis',(0.,-4.29586394988857E-10,-1.));
#8129=DIRECTION('center_axis',(1.,0.,0.));
#8130=DIRECTION('ref_axis',(0.,-4.29586394988857E-10,-1.));
#8131=DIRECTION('center_axis',(1.,4.17203725971588E-9,2.0031116033889E-18));
#8132=DIRECTION('ref_axis',(4.1720372752498E-9,-1.,5.66553889764798E-16));
#8133=DIRECTION('center_axis',(1.,4.17203725971588E-9,2.0031116033889E-18));
#8134=DIRECTION('ref_axis',(-4.17203725971588E-9,1.,5.39459847610519E-43));
#8135=DIRECTION('center_axis',(1.,1.53144334479515E-17,-1.9842828066192E-17));
#8136=DIRECTION('ref_axis',(-1.9842828066192E-17,0.,-1.));
#8137=DIRECTION('center_axis',(1.,0.,0.));
#8138=DIRECTION('ref_axis',(0.,0.,-1.));
#8139=DIRECTION('center_axis',(1.,6.36556116938371E-17,1.00386354793954E-17));
#8140=DIRECTION('ref_axis',(-6.3655612933414E-17,1.,0.));
#8141=DIRECTION('center_axis',(1.00386354793954E-17,1.22464679914735E-16,
-1.));
#8142=DIRECTION('ref_axis',(6.36556105223495E-17,-1.,-1.22464679914735E-16));
#8143=DIRECTION('center_axis',(1.,1.35504238326755E-16,2.34999225611352E-17));
#8144=DIRECTION('ref_axis',(-1.35504238326755E-16,1.,1.40763492406121E-49));
#8145=DIRECTION('center_axis',(1.,1.35504238326755E-16,2.34999225611352E-17));
#8146=DIRECTION('ref_axis',(-1.35504238326755E-16,1.,1.40763492406121E-49));
#8147=DIRECTION('center_axis',(1.,0.,0.));
#8148=DIRECTION('ref_axis',(0.,0.,-1.));
#8149=DIRECTION('center_axis',(-1.,0.,0.));
#8150=DIRECTION('ref_axis',(0.,-6.60206605267583E-10,1.));
#8151=DIRECTION('center_axis',(-1.,0.,0.));
#8152=DIRECTION('ref_axis',(0.,-6.60206605267583E-10,1.));
#8153=DIRECTION('',(1.,0.,0.));
#8154=DIRECTION('center_axis',(1.,0.,0.));
#8155=DIRECTION('ref_axis',(0.,0.,-1.));
#8156=DIRECTION('',(-1.,0.,0.));
#8157=DIRECTION('center_axis',(1.,0.,0.));
#8158=DIRECTION('ref_axis',(0.,0.,-1.));
#8159=DIRECTION('center_axis',(1.,1.18552772674719E-16,-1.97711088800387E-17));
#8160=DIRECTION('ref_axis',(-1.18552772074394E-16,1.,0.));
#8161=DIRECTION('center_axis',(-1.,0.,0.));
#8162=DIRECTION('ref_axis',(0.,-2.05103586755523E-10,1.));
#8163=DIRECTION('center_axis',(-1.97711088800387E-17,1.22464679914735E-16,
-1.));
#8164=DIRECTION('ref_axis',(1.18552771796194E-16,-1.,-1.22464679914735E-16));
#8165=DIRECTION('center_axis',(-1.,0.,0.));
#8166=DIRECTION('ref_axis',(0.,-2.05103586755523E-10,1.));
#8167=DIRECTION('center_axis',(-1.,2.92206431305708E-17,3.78610282642285E-17));
#8168=DIRECTION('ref_axis',(3.78610282642285E-17,0.,1.));
#8169=DIRECTION('center_axis',(1.,1.20795004338275E-8,6.525328094131E-17));
#8170=DIRECTION('ref_axis',(-1.20795004338275E-8,1.,4.44135209129409E-41));
#8171=DIRECTION('center_axis',(1.,-1.20794999078492E-8,-6.65136044666218E-17));
#8172=DIRECTION('ref_axis',(1.20794999078492E-8,1.,-3.20659696454606E-41));
#8173=DIRECTION('center_axis',(1.,0.,0.));
#8174=DIRECTION('ref_axis',(0.,0.,-1.));
#8175=DIRECTION('center_axis',(1.,0.,0.));
#8176=DIRECTION('ref_axis',(0.,0.,-1.));
#8177=DIRECTION('',(-1.,0.,0.));
#8178=DIRECTION('center_axis',(1.,-1.20794999078492E-8,-6.65136044666218E-17));
#8179=DIRECTION('ref_axis',(-1.20794999243885E-8,-1.,-5.21792575105832E-12));
#8180=DIRECTION('center_axis',(-3.90112644891662E-10,-1.,-3.90117034748036E-10));
#8181=DIRECTION('ref_axis',(-7.96162782272821E-7,3.90117345341081E-10,-0.999999999999683));
#8182=DIRECTION('center_axis',(1.,-1.20794992145421E-8,-4.8381018443521E-19));
#8183=DIRECTION('ref_axis',(1.48029741503464E-16,1.78300800621899E-8,-1.));
#8184=DIRECTION('center_axis',(-3.90083830404282E-10,-1.,3.90119162273478E-10));
#8185=DIRECTION('ref_axis',(-0.999999999999707,3.90084128868405E-10,7.65059156489968E-7));
#8186=DIRECTION('center_axis',(1.,1.20795004338275E-8,6.525328094131E-17));
#8187=DIRECTION('ref_axis',(-1.20795004609008E-8,1.,0.));
#8188=DIRECTION('center_axis',(1.,1.20795004338275E-8,6.525328094131E-17));
#8189=DIRECTION('ref_axis',(-1.20795004338275E-8,1.,4.44135209129409E-41));
#8190=DIRECTION('center_axis',(1.,2.92206431305708E-17,-3.78610282642285E-17));
#8191=DIRECTION('ref_axis',(-3.78610282642285E-17,0.,-1.));
#8192=DIRECTION('center_axis',(1.,-1.20794999071527E-8,2.28224857621035E-17));
#8193=DIRECTION('ref_axis',(1.20794999071527E-8,1.,-1.89856639006012E-41));
#8194=DIRECTION('center_axis',(1.,1.20794999172425E-8,-1.59545740616835E-17));
#8195=DIRECTION('ref_axis',(-1.20794999172425E-8,1.,2.99570552288603E-42));
#8196=DIRECTION('center_axis',(1.,0.,-1.15648231731787E-16));
#8197=DIRECTION('ref_axis',(-1.15648231731787E-16,0.,-1.));
#8198=DIRECTION('',(1.,0.,-1.15648231731787E-16));
#8199=DIRECTION('center_axis',(1.,0.,0.));
#8200=DIRECTION('ref_axis',(0.,-4.29586131949163E-10,-1.));
#8201=DIRECTION('center_axis',(1.,-1.20794999071527E-8,2.28224857621035E-17));
#8202=DIRECTION('ref_axis',(1.20794999071527E-8,1.,-1.89856639006012E-41));
#8203=DIRECTION('center_axis',(1.,1.20794999172425E-8,-1.59545740616835E-17));
#8204=DIRECTION('ref_axis',(1.20794999243885E-8,-1.,-8.2319592183107E-12));
#8205=DIRECTION('center_axis',(3.9010897446429E-10,-1.,-3.90108144056802E-10));
#8206=DIRECTION('ref_axis',(0.999999999999707,3.90109272919983E-10,-7.65059154471383E-7));
#8207=DIRECTION('center_axis',(3.90083837031876E-10,-1.,3.90119162425402E-10));
#8208=DIRECTION('ref_axis',(7.96162783282112E-7,3.90119472995512E-10,0.999999999999683));
#8209=DIRECTION('center_axis',(1.,-1.20794999071527E-8,2.28224857621035E-17));
#8210=DIRECTION('ref_axis',(1.20794999243885E-8,1.,0.));
#8211=DIRECTION('axis',(0.,0.,1.));
#8212=DIRECTION('refdir',(1.,0.,0.));
#8213=DIRECTION('axis',(0.,0.,1.));
#8214=DIRECTION('refdir',(1.,0.,0.));
#8215=DIRECTION('center_axis',(0.,0.992193411636613,-0.124708595954326));
#8216=DIRECTION('ref_axis',(0.,0.124708595954326,0.992193411636613));
#8217=DIRECTION('center_axis',(0.,0.992193411636613,-0.124708595954326));
#8218=DIRECTION('ref_axis',(0.,0.124708595954326,0.992193411636613));
#8219=DIRECTION('',(0.,0.992193411636613,-0.124708595954326));
#8220=DIRECTION('center_axis',(0.,0.992193411636613,-0.124708595954326));
#8221=DIRECTION('ref_axis',(0.,0.124708595954326,0.992193411636613));
#8222=DIRECTION('center_axis',(1.04435470755135E-16,0.992193408738347,-0.124708619013202));
#8223=DIRECTION('ref_axis',(9.66752478783401E-35,0.124708619013202,0.992193408738347));
#8224=DIRECTION('center_axis',(2.63594069435475E-16,0.992193411026652,-0.124708600807231));
#8225=DIRECTION('ref_axis',(-6.9705924208555E-34,0.124708600807231,0.992193411026652));
#8226=DIRECTION('center_axis',(0.,0.992193411636614,-0.124708595954319));
#8227=DIRECTION('ref_axis',(0.,0.124708595954319,0.992193411636613));
#8228=DIRECTION('center_axis',(0.,0.992193411636614,-0.124708595954319));
#8229=DIRECTION('ref_axis',(0.,0.124708595954319,0.992193411636613));
#8230=DIRECTION('center_axis',(0.,0.992193411636614,-0.124708595954319));
#8231=DIRECTION('ref_axis',(0.,0.124708595954319,0.992193411636613));
#8232=DIRECTION('',(0.,-0.992193411636613,0.124708595954319));
#8233=DIRECTION('center_axis',(2.38185692356041E-15,0.992193411026652,-0.124708600807233));
#8234=DIRECTION('ref_axis',(-6.67137153928239E-35,0.124708600807233,0.992193411026652));
#8235=DIRECTION('axis',(0.,0.,1.));
#8236=DIRECTION('refdir',(1.,0.,0.));
#8237=DIRECTION('center_axis',(0.,-0.99219341162106,0.124708596078064));
#8238=DIRECTION('ref_axis',(0.,-0.124708596078064,-0.99219341162106));
#8239=DIRECTION('center_axis',(0.,-0.99219341162106,0.124708596078064));
#8240=DIRECTION('ref_axis',(0.,-0.124708596078064,-0.99219341162106));
#8241=DIRECTION('center_axis',(0.,-0.99219341162106,0.124708596078064));
#8242=DIRECTION('ref_axis',(0.,-0.124708596078064,-0.99219341162106));
#8243=DIRECTION('center_axis',(0.,-0.99219341162106,0.124708596078064));
#8244=DIRECTION('ref_axis',(0.,-0.124708596078064,-0.99219341162106));
#8245=DIRECTION('center_axis',(0.,-0.99219341162106,0.124708596078064));
#8246=DIRECTION('ref_axis',(0.,-0.124708596078064,-0.99219341162106));
#8247=DIRECTION('',(0.,0.99219341162106,-0.124708596078064));
#8248=DIRECTION('center_axis',(0.,-0.99219341162106,0.124708596078064));
#8249=DIRECTION('ref_axis',(0.,-0.124708596078064,-0.99219341162106));
#8250=DIRECTION('center_axis',(0.,-0.99219341162106,0.124708596078064));
#8251=DIRECTION('ref_axis',(0.,-0.124708596078064,-0.99219341162106));
#8252=DIRECTION('center_axis',(0.,-0.99219341162106,0.124708596078064));
#8253=DIRECTION('ref_axis',(0.,-0.124708596078064,-0.99219341162106));
#8254=DIRECTION('center_axis',(0.,-0.99219341162106,0.124708596078064));
#8255=DIRECTION('ref_axis',(0.,-0.124708596078064,-0.99219341162106));
#8256=DIRECTION('center_axis',(-3.56161599407301E-15,-0.992193416380086,
0.124708558214796));
#8257=DIRECTION('ref_axis',(5.41945887256173E-32,-0.124708558214796,-0.992193416380086));
#8258=DIRECTION('center_axis',(9.14782393218023E-15,-0.992193507035639,
0.124707836948281));
#8259=DIRECTION('ref_axis',(-3.40310025056597E-32,-0.124707836948281,-0.992193507035639));
#8260=DIRECTION('',(1.,0.,0.));
#8261=DIRECTION('center_axis',(-2.03678483080916E-15,0.992193402544911,
-0.124708668288743));
#8262=DIRECTION('ref_axis',(4.13177645825422E-32,0.124708668288743,0.992193402544911));
#8263=DIRECTION('',(3.27320801842311E-8,-0.124708648640395,-0.992193405014509));
#8264=DIRECTION('',(1.,0.,0.));
#8265=DIRECTION('center_axis',(-8.81386107600706E-16,0.992193416883257,
-0.124708554211516));
#8266=DIRECTION('ref_axis',(7.20809393353264E-33,0.124708554211516,0.992193416883257));
#8267=DIRECTION('',(-1.,0.,0.));
#8268=DIRECTION('',(-1.81892028111732E-8,-0.124708565130038,-0.992193415510911));
#8269=DIRECTION('center_axis',(1.3069838162107E-15,-0.992193291960435,0.124709548105651));
#8270=DIRECTION('ref_axis',(-6.81953595921427E-33,-0.124709548105651,-0.992193291960435));
#8271=DIRECTION('',(-1.,0.,0.));
#8272=DIRECTION('center_axis',(-8.75485997098923E-16,0.992193416883257,
-0.124708554211516));
#8273=DIRECTION('ref_axis',(5.40831068588944E-33,0.124708554211516,0.992193416883257));
#8274=DIRECTION('',(-1.81892161321154E-8,0.124708565130016,0.992193415510914));
#8275=DIRECTION('',(-1.,0.,0.));
#8276=DIRECTION('center_axis',(-2.04304168492322E-15,0.992193402544911,
-0.124708668288743));
#8277=DIRECTION('ref_axis',(-3.57454093922697E-33,0.124708668288743,0.992193402544911));
#8278=DIRECTION('',(1.,0.,0.));
#8279=DIRECTION('',(3.27320408114478E-8,0.124708648640324,0.992193405014518));
#8280=DIRECTION('center_axis',(-4.36194494519598E-17,-0.124708594908011,
-0.992193411768124));
#8281=DIRECTION('ref_axis',(2.29865079049834E-34,0.992193411768124,-0.124708594908011));
#8282=DIRECTION('',(0.517637880127419,0.848920488901183,-0.106700649393379));
#8283=DIRECTION('',(-1.,0.,0.));
#8284=DIRECTION('',(0.517637880127419,-0.848920488901183,0.106700649393379));
#8285=DIRECTION('center_axis',(-0.855599804264349,-0.513596894340652,0.0645538927288335));
#8286=DIRECTION('ref_axis',(0.514670382381903,-0.857388125354478,2.04082986758841E-17));
#8287=DIRECTION('',(-6.44853564777329E-9,0.124708601376938,0.992193410955046));
#8288=DIRECTION('',(0.51763788012742,-0.848920488901183,0.106700649393376));
#8289=DIRECTION('center_axis',(3.7067617295265E-17,-0.124708594908011,-0.992193411768124));
#8290=DIRECTION('ref_axis',(8.52848234808661E-35,0.992193411768124,-0.124708594908011));
#8291=DIRECTION('',(-1.,0.,0.));
#8292=DIRECTION('',(0.517637880127419,0.848920488901183,-0.106700649393379));
#8293=DIRECTION('center_axis',(-0.855599804264349,0.513596894340652,-0.0645538927288335));
#8294=DIRECTION('ref_axis',(-0.514670382381903,-0.857388125354478,2.04082986758841E-17));
#8295=DIRECTION('',(6.44853327929739E-9,0.124708601376938,0.992193410955046));
#8296=DIRECTION('center_axis',(-1.20013551743046E-17,0.992193410955045,
-0.12470860137694));
#8297=DIRECTION('ref_axis',(4.64258476562535E-35,0.12470860137694,0.992193410955045));
#8298=DIRECTION('axis',(0.,0.,1.));
#8299=DIRECTION('refdir',(1.,0.,0.));
#8300=DIRECTION('center_axis',(0.,-0.388095893070246,0.921618998166817));
#8301=DIRECTION('ref_axis',(0.,-0.921618998166817,-0.388095893070246));
#8302=DIRECTION('center_axis',(0.,-0.388095893070246,0.921618998166817));
#8303=DIRECTION('ref_axis',(0.,-0.921618998166817,-0.388095893070246));
#8304=DIRECTION('',(0.,-0.388095893070246,0.921618998166817));
#8305=DIRECTION('center_axis',(0.,-0.388095893070246,0.921618998166817));
#8306=DIRECTION('ref_axis',(0.,-0.921618998166817,-0.388095893070246));
#8307=DIRECTION('center_axis',(-2.17338651928477E-15,-0.388095852305961,
0.921619015332751));
#8308=DIRECTION('ref_axis',(1.42974172085408E-32,-0.921619015332751,-0.388095852305961));
#8309=DIRECTION('center_axis',(3.34334487188163E-15,-0.388095889853545,
0.921618999521378));
#8310=DIRECTION('ref_axis',(4.30883609996747E-32,-0.921618999521378,-0.388095889853545));
#8311=DIRECTION('center_axis',(0.,-0.388095893070248,0.921618998166817));
#8312=DIRECTION('ref_axis',(0.,-0.921618998166816,-0.388095893070248));
#8313=DIRECTION('center_axis',(0.,-0.388095893070248,0.921618998166817));
#8314=DIRECTION('ref_axis',(0.,-0.921618998166816,-0.388095893070248));
#8315=DIRECTION('center_axis',(0.,-0.388095893070248,0.921618998166817));
#8316=DIRECTION('ref_axis',(0.,-0.921618998166816,-0.388095893070248));
#8317=DIRECTION('',(0.,0.388095893070248,-0.921618998166817));
#8318=DIRECTION('center_axis',(9.77214352076555E-16,-0.388095865559816,
0.921619009751523));
#8319=DIRECTION('ref_axis',(1.19984570551963E-32,-0.921619009751523,-0.388095865559816));
#8320=DIRECTION('axis',(0.,0.,1.));
#8321=DIRECTION('refdir',(1.,0.,0.));
#8322=DIRECTION('center_axis',(0.,0.604097518614064,0.796910401490865));
#8323=DIRECTION('ref_axis',(0.,-0.796910401490865,0.604097518614064));
#8324=DIRECTION('center_axis',(0.,0.604097518614064,0.796910401490865));
#8325=DIRECTION('ref_axis',(0.,-0.796910401490865,0.604097518614064));
#8326=DIRECTION('center_axis',(0.,0.604097518614064,0.796910401490865));
#8327=DIRECTION('ref_axis',(0.,-0.796910401490865,0.604097518614064));
#8328=DIRECTION('center_axis',(0.,0.604097518614064,0.796910401490865));
#8329=DIRECTION('ref_axis',(0.,-0.796910401490865,0.604097518614064));
#8330=DIRECTION('center_axis',(0.,0.604097518614064,0.796910401490865));
#8331=DIRECTION('ref_axis',(0.,-0.796910401490865,0.604097518614064));
#8332=DIRECTION('',(0.,-0.604097518614064,-0.796910401490865));
#8333=DIRECTION('center_axis',(0.,0.604097518614064,0.796910401490865));
#8334=DIRECTION('ref_axis',(0.,-0.796910401490865,0.604097518614064));
#8335=DIRECTION('center_axis',(0.,0.604097518614064,0.796910401490865));
#8336=DIRECTION('ref_axis',(0.,-0.796910401490865,0.604097518614064));
#8337=DIRECTION('center_axis',(0.,0.604097518614064,0.796910401490865));
#8338=DIRECTION('ref_axis',(0.,-0.796910401490865,0.604097518614064));
#8339=DIRECTION('center_axis',(0.,0.604097518614064,0.796910401490865));
#8340=DIRECTION('ref_axis',(0.,-0.796910401490865,0.604097518614064));
#8341=DIRECTION('center_axis',(1.76011166144385E-16,0.604097524343638,0.796910397147564));
#8342=DIRECTION('ref_axis',(-5.69382634799286E-34,-0.796910397147564,0.604097524343638));
#8343=DIRECTION('center_axis',(-2.4695605328884E-15,0.604097388004457,0.796910500499393));
#8344=DIRECTION('ref_axis',(-2.15217716924996E-31,-0.796910500499393,0.604097388004457));
#8345=DIRECTION('',(1.,0.,0.));
#8346=DIRECTION('center_axis',(5.0257917292328E-15,-0.604097535980688,-0.796910388326104));
#8347=DIRECTION('ref_axis',(3.96880149093465E-31,0.796910388326104,-0.604097535980688));
#8348=DIRECTION('',(9.06795873383563E-9,-0.796910391640021,0.60409753160905));
#8349=DIRECTION('',(1.,0.,0.));
#8350=DIRECTION('center_axis',(-1.3539365332793E-15,-0.604097535980685,
-0.796910388326106));
#8351=DIRECTION('ref_axis',(-3.09014762786369E-33,0.796910388326106,-0.604097535980685));
#8352=DIRECTION('',(-1.,0.,0.));
#8353=DIRECTION('',(9.06765857867901E-9,-0.796910391640318,0.60409753160866));
#8354=DIRECTION('center_axis',(1.30898403527359E-14,0.604097388004449,0.796910500499399));
#8355=DIRECTION('ref_axis',(7.65782089424487E-31,-0.796910500499399,0.604097388004449));
#8356=DIRECTION('',(-1.,1.78664147484789E-13,0.));
#8357=DIRECTION('center_axis',(-1.36705691295974E-15,-0.604097535980685,
-0.796910388326106));
#8358=DIRECTION('ref_axis',(-4.01110836398031E-32,0.796910388326106,-0.604097535980685));
#8359=DIRECTION('',(9.06797358508429E-9,0.796910391640005,-0.604097531609072));
#8360=DIRECTION('',(-1.,0.,0.));
#8361=DIRECTION('center_axis',(2.86322345620586E-16,-0.604097535980689,
-0.796910388326103));
#8362=DIRECTION('ref_axis',(4.76719382107084E-33,0.796910388326103,-0.604097535980689));
#8363=DIRECTION('',(1.,0.,0.));
#8364=DIRECTION('',(9.06768872847231E-9,0.796910391640293,-0.604097531608692));
#8365=DIRECTION('center_axis',(1.49607962990053E-17,-0.796910402395455,
0.604097517420751));
#8366=DIRECTION('ref_axis',(6.62628247037524E-34,-0.604097517420751,-0.796910402395455));
#8367=DIRECTION('',(0.517637881323564,-0.516865717224615,-0.68183638372907));
#8368=DIRECTION('',(-1.,0.,0.));
#8369=DIRECTION('',(0.517637881323564,0.516865717224616,0.68183638372907));
#8370=DIRECTION('center_axis',(-0.855599803540681,0.312703760192046,0.412511011420185));
#8371=DIRECTION('ref_axis',(0.434290367983341,3.1478940293141E-16,0.900772932695524));
#8372=DIRECTION('',(-6.812600991711E-9,0.796910393860769,-0.604097528679495));
#8373=DIRECTION('',(0.517637881323564,0.516865717224607,0.681836383729077));
#8374=DIRECTION('center_axis',(2.02339551431575E-18,-0.796910402395456,
0.60409751742075));
#8375=DIRECTION('ref_axis',(2.11465894662532E-34,-0.60409751742075,-0.796910402395456));
#8376=DIRECTION('',(-1.,0.,0.));
#8377=DIRECTION('',(0.517637881323564,-0.516865717224604,-0.681836383729078));
#8378=DIRECTION('center_axis',(-0.855599803540681,-0.312703760192046,-0.412511011420185));
#8379=DIRECTION('ref_axis',(-0.434290367983341,3.1478940293141E-16,0.900772932695524));
#8380=DIRECTION('',(6.812600991711E-9,0.796910393860769,-0.604097528679495));
#8381=DIRECTION('center_axis',(-4.61706709228339E-17,-0.604097528679492,
-0.796910393860772));
#8382=DIRECTION('ref_axis',(-3.71158212193438E-33,0.796910393860772,-0.604097528679492));
#8383=DIRECTION('axis',(0.,0.,1.));
#8384=DIRECTION('refdir',(1.,0.,0.));
#8385=DIRECTION('center_axis',(0.,0.388095893919631,-0.92161899780914));
#8386=DIRECTION('ref_axis',(0.,0.921618997809139,0.388095893919631));
#8387=DIRECTION('center_axis',(0.,0.388095893919631,-0.92161899780914));
#8388=DIRECTION('ref_axis',(0.,0.921618997809139,0.388095893919631));
#8389=DIRECTION('center_axis',(0.,0.388095893919631,-0.92161899780914));
#8390=DIRECTION('ref_axis',(0.,0.921618997809139,0.388095893919631));
#8391=DIRECTION('center_axis',(0.,0.388095893919631,-0.92161899780914));
#8392=DIRECTION('ref_axis',(0.,0.921618997809139,0.388095893919631));
#8393=DIRECTION('center_axis',(0.,0.388095893919631,-0.92161899780914));
#8394=DIRECTION('ref_axis',(0.,0.921618997809139,0.388095893919631));
#8395=DIRECTION('',(0.,-0.388095893919631,0.921618997809139));
#8396=DIRECTION('center_axis',(0.,0.388095893919631,-0.92161899780914));
#8397=DIRECTION('ref_axis',(0.,0.921618997809139,0.388095893919631));
#8398=DIRECTION('center_axis',(0.,0.388095893919631,-0.92161899780914));
#8399=DIRECTION('ref_axis',(0.,0.921618997809139,0.388095893919631));
#8400=DIRECTION('center_axis',(0.,0.388095893919631,-0.92161899780914));
#8401=DIRECTION('ref_axis',(0.,0.921618997809139,0.388095893919631));
#8402=DIRECTION('center_axis',(0.,0.388095893919631,-0.92161899780914));
#8403=DIRECTION('ref_axis',(0.,0.921618997809139,0.388095893919631));
#8404=DIRECTION('center_axis',(1.75398457025153E-15,0.388095852305965,-0.921619015332749));
#8405=DIRECTION('ref_axis',(3.06157850855551E-32,0.921619015332749,0.388095852305965));
#8406=DIRECTION('center_axis',(2.26659755541862E-15,0.388095750770971,-0.921619058089359));
#8407=DIRECTION('ref_axis',(3.64804420840904E-32,0.921619058089359,0.388095750770971));
#8408=DIRECTION('',(1.,0.,0.));
#8409=DIRECTION('center_axis',(2.22848289163665E-15,-0.388095804062443,
0.921619035648204));
#8410=DIRECTION('ref_axis',(-1.35081649158113E-31,-0.921619035648204,-0.388095804062443));
#8411=DIRECTION('',(4.2446461003979E-8,0.921619025681862,0.388095827729717));
#8412=DIRECTION('',(1.,0.,0.));
#8413=DIRECTION('center_axis',(-1.49720831504864E-15,-0.388095851468213,
0.921619015685529));
#8414=DIRECTION('ref_axis',(-1.5492957769102E-32,-0.921619015685529,-0.388095851468213));
#8415=DIRECTION('',(-1.,0.,0.));
#8416=DIRECTION('',(1.96652829206634E-8,0.921619011068175,0.388095862433136));
#8417=DIRECTION('center_axis',(-8.05371050902293E-15,0.388095039684462,
-0.921619357529081));
#8418=DIRECTION('ref_axis',(-4.42778246385967E-33,0.921619357529081,0.388095039684462));
#8419=DIRECTION('',(-1.,0.,0.));
#8420=DIRECTION('center_axis',(-1.48913479951885E-15,-0.388095851468213,
0.921619015685529));
#8421=DIRECTION('ref_axis',(3.33947309911167E-32,-0.921619015685529,-0.388095851468213));
#8422=DIRECTION('',(1.96652829206634E-8,-0.921619011068175,-0.388095862433136));
#8423=DIRECTION('',(-1.,0.,0.));
#8424=DIRECTION('center_axis',(2.25639593240362E-15,-0.388095804062443,
0.921619035648204));
#8425=DIRECTION('ref_axis',(-1.14895763187271E-31,-0.921619035648204,-0.388095804062443));
#8426=DIRECTION('',(1.,0.,0.));
#8427=DIRECTION('',(4.2446461003979E-8,-0.921619025681862,-0.388095827729717));
#8428=DIRECTION('center_axis',(4.13124616662422E-17,0.921618997376154,0.388095894947849));
#8429=DIRECTION('ref_axis',(-4.90455258387228E-34,-0.388095894947849,0.921618997376154));
#8430=DIRECTION('',(0.517637880705175,-0.332054771617521,0.788537033439198));
#8431=DIRECTION('',(-1.,0.,0.));
#8432=DIRECTION('',(0.517637880705175,0.332054771617521,-0.788537033439198));
#8433=DIRECTION('center_axis',(-0.855599803914806,0.200893135247141,-0.477064905176978));
#8434=DIRECTION('ref_axis',(-0.486993155484724,-9.98976039519683E-17,0.873405785709616));
#8435=DIRECTION('',(-6.49786640054161E-9,-0.921618997845643,-0.388095893832946));
#8436=DIRECTION('',(0.517637880705176,0.332054769800693,-0.788537034204268));
#8437=DIRECTION('center_axis',(-1.84726342759314E-17,0.921618998270346,
0.388095892824394));
#8438=DIRECTION('ref_axis',(3.04412378032587E-35,-0.388095892824394,0.921618998270346));
#8439=DIRECTION('',(-1.,0.,0.));
#8440=DIRECTION('',(0.517637880705175,-0.332054769800693,0.788537034204268));
#8441=DIRECTION('center_axis',(-0.855599803914806,-0.200893135247141,0.477064905176978));
#8442=DIRECTION('ref_axis',(0.486993155484724,-9.98976039519683E-17,0.873405785709616));
#8443=DIRECTION('',(6.49786640054161E-9,-0.921618997845643,-0.388095893832946));
#8444=DIRECTION('center_axis',(8.66968723023857E-18,-0.388095893832947,
0.921618997845642));
#8445=DIRECTION('ref_axis',(-1.74143232952537E-34,-0.921618997845642,-0.388095893832947));
#8446=DIRECTION('axis',(0.,0.,1.));
#8447=DIRECTION('refdir',(1.,0.,0.));
#8448=DIRECTION('center_axis',(0.,-0.604097518460404,-0.796910401607346));
#8449=DIRECTION('ref_axis',(0.,0.796910401607346,-0.604097518460404));
#8450=DIRECTION('center_axis',(0.,-0.604097518460404,-0.796910401607346));
#8451=DIRECTION('ref_axis',(0.,0.796910401607346,-0.604097518460404));
#8452=DIRECTION('',(0.,-0.604097518460404,-0.796910401607346));
#8453=DIRECTION('center_axis',(0.,-0.604097518460404,-0.796910401607346));
#8454=DIRECTION('ref_axis',(0.,0.796910401607346,-0.604097518460404));
#8455=DIRECTION('center_axis',(-1.20725909381357E-16,-0.6040974946122,-0.796910419685465));
#8456=DIRECTION('ref_axis',(7.15152886696226E-32,0.796910419685465,-0.6040974946122));
#8457=DIRECTION('center_axis',(6.24224782272207E-17,-0.604097506757326,
-0.796910410478859));
#8458=DIRECTION('ref_axis',(-1.64388262168888E-33,0.796910410478859,-0.604097506757326));
#8459=DIRECTION('center_axis',(0.,-0.604097518460408,-0.796910401607343));
#8460=DIRECTION('ref_axis',(0.,0.796910401607343,-0.604097518460408));
#8461=DIRECTION('center_axis',(0.,-0.604097518460408,-0.796910401607343));
#8462=DIRECTION('ref_axis',(0.,0.796910401607343,-0.604097518460408));
#8463=DIRECTION('center_axis',(0.,-0.604097518460408,-0.796910401607343));
#8464=DIRECTION('ref_axis',(0.,0.796910401607343,-0.604097518460408));
#8465=DIRECTION('',(0.,0.604097518460408,0.796910401607343));
#8466=DIRECTION('center_axis',(-2.35801524345747E-16,-0.604097538134134,
-0.796910386693685));
#8467=DIRECTION('ref_axis',(2.53292576583338E-33,0.796910386693685,-0.604097538134134));
#8468=DIRECTION('axis',(0.,0.,1.));
#8469=DIRECTION('refdir',(1.,0.,0.));
#8470=DIRECTION('center_axis',(-1.,0.,0.));
#8471=DIRECTION('ref_axis',(0.,0.464060113818661,0.885803708934779));
#8472=DIRECTION('center_axis',(1.,-1.0700065104041E-8,5.60561397559687E-9));
#8473=DIRECTION('ref_axis',(1.48029741503464E-16,-0.464060114221788,-0.885803708723587));
#8474=DIRECTION('',(-1.,0.,0.));
#8475=DIRECTION('center_axis',(1.,0.,0.));
#8476=DIRECTION('ref_axis',(0.,-0.464060130396268,-0.885803700250004));
#8477=DIRECTION('center_axis',(1.,0.,0.));
#8478=DIRECTION('ref_axis',(0.,-0.464060130396268,-0.885803700250004));
#8479=DIRECTION('center_axis',(1.,-1.0700065104041E-8,5.60561397559687E-9));
#8480=DIRECTION('ref_axis',(1.48029741503464E-16,-0.464060114221788,-0.885803708723587));
#8481=DIRECTION('center_axis',(-1.,0.,0.));
#8482=DIRECTION('ref_axis',(0.,0.464060113818661,0.885803708934779));
#8483=DIRECTION('center_axis',(1.,0.,0.));
#8484=DIRECTION('ref_axis',(0.,0.464060113818661,0.885803708934779));
#8485=DIRECTION('',(-1.,0.,0.));
#8486=DIRECTION('center_axis',(1.,0.,0.));
#8487=DIRECTION('ref_axis',(0.,-0.464060130396268,-0.885803700250004));
#8488=DIRECTION('center_axis',(1.,0.,0.));
#8489=DIRECTION('ref_axis',(0.,-0.464060130396268,-0.885803700250004));
#8490=DIRECTION('center_axis',(-1.,0.,0.));
#8491=DIRECTION('ref_axis',(0.,0.464060113818661,0.885803708934779));
#8492=DIRECTION('center_axis',(1.,-1.0700065104041E-8,5.60561397559687E-9));
#8493=DIRECTION('ref_axis',(1.48029741503464E-16,-0.464060114221788,-0.885803708723587));
#8494=DIRECTION('',(-1.,0.,0.));
#8495=DIRECTION('center_axis',(-1.,3.00553233246224E-15,2.27067042532096E-15));
#8496=DIRECTION('ref_axis',(0.,0.464060113818661,0.885803708934779));
#8497=DIRECTION('center_axis',(1.,-1.0700065104041E-8,5.60561397559687E-9));
#8498=DIRECTION('ref_axis',(1.48029741503464E-16,-0.464060114221788,-0.885803708723587));
#8499=DIRECTION('center_axis',(1.,0.,0.));
#8500=DIRECTION('ref_axis',(0.,-0.464060145800476,-0.885803692179955));
#8501=DIRECTION('center_axis',(1.,0.,0.));
#8502=DIRECTION('ref_axis',(0.,-0.464060130396268,-0.885803700250004));
#8503=DIRECTION('',(1.,0.,0.));
#8504=DIRECTION('center_axis',(1.,0.,0.));
#8505=DIRECTION('ref_axis',(0.,-0.464060145800476,-0.885803692179955));
#8506=DIRECTION('center_axis',(1.,0.,0.));
#8507=DIRECTION('ref_axis',(0.,-0.464060145800476,-0.885803692179955));
#8508=DIRECTION('center_axis',(-1.,0.,0.));
#8509=DIRECTION('ref_axis',(0.,-0.464060145800476,-0.885803692179955));
#8510=DIRECTION('',(1.,0.,0.));
#8511=DIRECTION('center_axis',(1.,-1.0700065104041E-8,5.60561397559687E-9));
#8512=DIRECTION('ref_axis',(1.48029741503464E-16,-0.464060114221788,-0.885803708723587));
#8513=DIRECTION('center_axis',(1.,8.31396011574228E-18,-4.70975743895875E-17));
#8514=DIRECTION('ref_axis',(-3.78610282642285E-17,-0.464060130015739,-0.885803700449358));
#8515=DIRECTION('center_axis',(1.,0.,0.));
#8516=DIRECTION('ref_axis',(0.,0.,-1.));
#8517=DIRECTION('center_axis',(1.,-5.36677334535434E-17,-1.02441631618442E-16));
#8518=DIRECTION('ref_axis',(-1.15648231731787E-16,-0.464060130015739,-0.885803700449358));
#8519=DIRECTION('',(-1.,5.36677334535434E-17,1.02441631618442E-16));
#8520=DIRECTION('center_axis',(1.,0.,0.));
#8521=DIRECTION('ref_axis',(0.,0.,-1.));
#8522=DIRECTION('center_axis',(-1.,0.,0.));
#8523=DIRECTION('ref_axis',(0.,0.,-1.));
#8524=DIRECTION('',(-1.,0.,0.));
#8525=DIRECTION('center_axis',(1.,-5.36677334535434E-17,-1.02441631618442E-16));
#8526=DIRECTION('ref_axis',(-1.15648231731787E-16,-0.464060130015739,-0.885803700449358));
#8527=DIRECTION('',(-1.,5.36677334535434E-17,1.02441631618442E-16));
#8528=DIRECTION('center_axis',(-1.,4.34535475133972E-17,1.99773034889551E-17));
#8529=DIRECTION('ref_axis',(3.78610282642285E-17,0.464060130015739,0.885803700449358));
#8530=DIRECTION('center_axis',(1.,-5.36677334535434E-17,-1.02441631618442E-16));
#8531=DIRECTION('ref_axis',(-1.15648231731787E-16,-0.464060130015739,-0.885803700449358));
#8532=DIRECTION('',(-1.,5.36677334535434E-17,1.02441631618442E-16));
#8533=DIRECTION('center_axis',(-1.,3.00553233246224E-15,2.27067042532096E-15));
#8534=DIRECTION('ref_axis',(-3.00553233246224E-15,-1.,4.51258949388147E-46));
#8535=DIRECTION('center_axis',(1.,0.,0.));
#8536=DIRECTION('ref_axis',(0.,0.,-1.));
#8537=DIRECTION('',(0.,-0.464060130015739,0.885803700449358));
#8538=DIRECTION('',(1.,0.,0.));
#8539=DIRECTION('',(0.,-0.464060130015739,0.885803700449358));
#8540=DIRECTION('',(1.,0.,0.));
#8541=DIRECTION('',(0.,-0.464060130015739,0.885803700449358));
#8542=DIRECTION('',(1.,0.,0.));
#8543=DIRECTION('',(0.,-0.464060130015739,0.885803700449358));
#8544=DIRECTION('',(1.,0.,0.));
#8545=DIRECTION('',(0.,-0.464060130015739,0.885803700449358));
#8546=DIRECTION('',(1.,0.,0.));
#8547=DIRECTION('',(0.,-0.464060130015739,0.885803700449358));
#8548=DIRECTION('',(1.,0.,0.));
#8549=DIRECTION('',(0.,-0.464060130015739,0.885803700449358));
#8550=DIRECTION('',(1.,0.,0.));
#8551=DIRECTION('axis',(0.,0.,1.));
#8552=DIRECTION('refdir',(1.,0.,0.));
#8553=DIRECTION('center_axis',(1.,0.,0.));
#8554=DIRECTION('ref_axis',(0.,0.,-1.));
#8555=DIRECTION('center_axis',(1.,0.,0.));
#8556=DIRECTION('ref_axis',(0.,0.,-1.));
#8557=DIRECTION('',(1.,0.,0.));
#8558=DIRECTION('center_axis',(1.,0.,0.));
#8559=DIRECTION('ref_axis',(0.,0.,-1.));
#8560=DIRECTION('center_axis',(-1.,0.,0.));
#8561=DIRECTION('ref_axis',(0.,0.,1.));
#8562=DIRECTION('',(0.,0.,1.));
#8563=DIRECTION('',(0.,-1.,0.));
#8564=DIRECTION('',(0.,0.,-1.));
#8565=DIRECTION('',(0.,1.,0.));
#8566=DIRECTION('center_axis',(1.,0.,-2.22044604925031E-14));
#8567=DIRECTION('ref_axis',(-2.22044604925031E-14,0.,-1.));
#8568=DIRECTION('center_axis',(1.,0.,-2.22044604925031E-14));
#8569=DIRECTION('ref_axis',(-2.22044604925031E-14,0.,-1.));
#8570=DIRECTION('center_axis',(-1.,0.,0.));
#8571=DIRECTION('ref_axis',(0.,0.,1.));
#8572=DIRECTION('center_axis',(-1.,0.,0.));
#8573=DIRECTION('ref_axis',(0.,0.,1.));
#8574=DIRECTION('center_axis',(-1.,0.,0.));
#8575=DIRECTION('ref_axis',(0.,0.,1.));
#8576=DIRECTION('center_axis',(-1.,0.,0.));
#8577=DIRECTION('ref_axis',(0.,0.,1.));
#8578=DIRECTION('center_axis',(1.,0.,-2.22044604925031E-14));
#8579=DIRECTION('ref_axis',(-2.22044604925031E-14,0.,-1.));
#8580=DIRECTION('center_axis',(1.,0.,-2.22044604925031E-14));
#8581=DIRECTION('ref_axis',(-2.22044604925031E-14,0.,-1.));
#8582=DIRECTION('center_axis',(-1.,-2.40737135441678E-17,-6.64151273659692E-18));
#8583=DIRECTION('ref_axis',(2.40737135441678E-17,-1.,8.32842834445041E-51));
#8584=DIRECTION('',(0.,1.,0.));
#8585=DIRECTION('',(0.,0.,-1.));
#8586=DIRECTION('',(0.,-1.,0.));
#8587=DIRECTION('',(0.,-0.74983784571108,0.66162164802806));
#8588=DIRECTION('',(0.,-1.,0.));
#8589=DIRECTION('',(0.,0.,1.));
#8590=DIRECTION('',(0.,-1.,0.));
#8591=DIRECTION('',(0.,0.,1.));
#8592=DIRECTION('center_axis',(1.,0.,-2.22044604925031E-14));
#8593=DIRECTION('ref_axis',(-2.22044604925031E-14,0.,-1.));
#8594=DIRECTION('center_axis',(1.,0.,-2.22044604925031E-14));
#8595=DIRECTION('ref_axis',(-2.22044604925031E-14,0.,-1.));
#8596=DIRECTION('center_axis',(-1.,0.,0.));
#8597=DIRECTION('ref_axis',(0.,0.,1.));
#8598=DIRECTION('center_axis',(-1.,0.,0.));
#8599=DIRECTION('ref_axis',(0.,0.,1.));
#8600=DIRECTION('center_axis',(-1.,0.,0.));
#8601=DIRECTION('ref_axis',(0.,0.,1.));
#8602=DIRECTION('center_axis',(-1.,0.,0.));
#8603=DIRECTION('ref_axis',(0.,0.,1.));
#8604=DIRECTION('center_axis',(1.,0.,-2.22044604925031E-14));
#8605=DIRECTION('ref_axis',(-2.22044604925031E-14,0.,-1.));
#8606=DIRECTION('center_axis',(1.,0.,-2.22044604925031E-14));
#8607=DIRECTION('ref_axis',(-2.22044604925031E-14,0.,-1.));
#8608=DIRECTION('center_axis',(1.,0.,-2.22044604925031E-14));
#8609=DIRECTION('ref_axis',(-2.22044604925031E-14,0.,-1.));
#8610=DIRECTION('',(1.,0.,-2.22044604925031E-14));
#8611=DIRECTION('center_axis',(1.,0.,-2.22044604925031E-14));
#8612=DIRECTION('ref_axis',(-2.22044604925031E-14,0.,-1.));
#8613=DIRECTION('',(1.,0.,-2.22044604925031E-14));
#8614=DIRECTION('center_axis',(-1.,0.,0.));
#8615=DIRECTION('ref_axis',(0.,0.,1.));
#8616=DIRECTION('',(-1.,0.,0.));
#8617=DIRECTION('center_axis',(-1.,0.,0.));
#8618=DIRECTION('ref_axis',(0.,0.,1.));
#8619=DIRECTION('',(-1.,0.,0.));
#8620=DIRECTION('center_axis',(-1.,0.,0.));
#8621=DIRECTION('ref_axis',(0.,0.,1.));
#8622=DIRECTION('',(-1.,0.,0.));
#8623=DIRECTION('center_axis',(-1.,0.,0.));
#8624=DIRECTION('ref_axis',(0.,0.,1.));
#8625=DIRECTION('',(-1.,0.,0.));
#8626=DIRECTION('center_axis',(1.,0.,-2.22044604925031E-14));
#8627=DIRECTION('ref_axis',(-2.22044604925031E-14,0.,-1.));
#8628=DIRECTION('',(1.,0.,-2.22044604925031E-14));
#8629=DIRECTION('center_axis',(1.,0.,-2.22044604925031E-14));
#8630=DIRECTION('ref_axis',(-2.22044604925031E-14,0.,-1.));
#8631=DIRECTION('',(1.,0.,-2.22044604925031E-14));
#8632=DIRECTION('center_axis',(0.,0.,1.));
#8633=DIRECTION('ref_axis',(1.,0.,0.));
#8634=DIRECTION('',(0.,-1.,0.));
#8635=DIRECTION('',(-1.,0.,0.));
#8636=DIRECTION('',(0.,1.,0.));
#8637=DIRECTION('',(-1.,0.,0.));
#8638=DIRECTION('',(-1.,0.,0.));
#8639=DIRECTION('',(1.,0.,0.));
#8640=DIRECTION('center_axis',(-7.13714802145194E-16,-1.,3.40997071849065E-18));
#8641=DIRECTION('ref_axis',(1.,-7.13714802145194E-16,0.));
#8642=DIRECTION('',(-1.,0.,0.));
#8643=DIRECTION('center_axis',(0.,0.,-1.));
#8644=DIRECTION('ref_axis',(-1.,0.,0.));
#8645=DIRECTION('',(-1.,0.,0.));
#8646=DIRECTION('center_axis',(-7.13714801545295E-18,1.,-3.40997071849065E-18));
#8647=DIRECTION('ref_axis',(-1.,-7.13714801545295E-18,0.));
#8648=DIRECTION('',(1.,0.,0.));
#8649=DIRECTION('',(0.,0.,-1.));
#8650=DIRECTION('',(1.,0.,0.));
#8651=DIRECTION('',(0.,0.,1.));
#8652=DIRECTION('center_axis',(0.,0.,-1.));
#8653=DIRECTION('ref_axis',(-1.,0.,0.));
#8654=DIRECTION('',(1.,0.,0.));
#8655=DIRECTION('',(0.,1.,0.));
#8656=DIRECTION('center_axis',(1.65076892874297E-17,1.,1.19112403377503E-17));
#8657=DIRECTION('ref_axis',(-1.,1.65076892874297E-17,0.));
#8658=DIRECTION('',(-1.,0.,0.));
#8659=DIRECTION('',(0.,0.,1.));
#8660=DIRECTION('center_axis',(-4.85520273159583E-18,-2.05298137436571E-17,
1.));
#8661=DIRECTION('ref_axis',(0.,-1.,-2.05298137436571E-17));
#8662=DIRECTION('',(-1.,0.,0.));
#8663=DIRECTION('',(0.,-1.,0.));
#8664=DIRECTION('center_axis',(-4.02545654738892E-18,0.661621648028061,
0.74983784571108));
#8665=DIRECTION('ref_axis',(-1.44095358341707E-35,-0.74983784571108,0.661621648028061));
#8666=DIRECTION('',(0.,-0.74983784571111,0.661621648028026));
#8667=DIRECTION('center_axis',(-7.13714801246482E-16,-1.,3.40997071849065E-18));
#8668=DIRECTION('ref_axis',(1.,-7.13714801246482E-16,0.));
#8669=DIRECTION('',(-1.,0.,0.));
#8670=DIRECTION('',(0.,0.,1.));
#8671=DIRECTION('',(0.,0.,-1.));
#8672=DIRECTION('center_axis',(-1.,2.40737135441678E-17,6.64151273659692E-18));
#8673=DIRECTION('ref_axis',(-2.40737135441678E-17,-1.,8.32842834445041E-51));
#8674=DIRECTION('',(0.,1.,0.));
#8675=DIRECTION('center_axis',(1.,0.,0.));
#8676=DIRECTION('ref_axis',(0.,0.,-1.));
#8677=DIRECTION('center_axis',(1.,0.,0.));
#8678=DIRECTION('ref_axis',(0.,0.,-1.));
#8679=DIRECTION('center_axis',(1.,0.,0.));
#8680=DIRECTION('ref_axis',(0.,0.,-1.));
#8681=DIRECTION('center_axis',(-1.,0.,0.));
#8682=DIRECTION('ref_axis',(0.,0.,1.));
#8683=DIRECTION('center_axis',(-1.,0.,0.));
#8684=DIRECTION('ref_axis',(0.,0.,1.));
#8685=DIRECTION('center_axis',(-1.,0.,0.));
#8686=DIRECTION('ref_axis',(0.,0.,1.));
#8687=DIRECTION('center_axis',(-1.,0.,0.));
#8688=DIRECTION('ref_axis',(0.,0.,1.));
#8689=DIRECTION('center_axis',(1.,0.,0.));
#8690=DIRECTION('ref_axis',(0.,0.,-1.));
#8691=DIRECTION('center_axis',(1.,0.,0.));
#8692=DIRECTION('ref_axis',(0.,0.,-1.));
#8693=DIRECTION('center_axis',(-1.,0.,0.));
#8694=DIRECTION('ref_axis',(0.,0.,1.));
#8695=DIRECTION('',(0.,1.,0.));
#8696=DIRECTION('center_axis',(1.,0.,0.));
#8697=DIRECTION('ref_axis',(0.,0.,-1.));
#8698=DIRECTION('center_axis',(1.,0.,0.));
#8699=DIRECTION('ref_axis',(0.,0.,-1.));
#8700=DIRECTION('center_axis',(1.,0.,0.));
#8701=DIRECTION('ref_axis',(0.,0.,-1.));
#8702=DIRECTION('center_axis',(-1.,0.,0.));
#8703=DIRECTION('ref_axis',(0.,0.,1.));
#8704=DIRECTION('center_axis',(-1.,0.,0.));
#8705=DIRECTION('ref_axis',(0.,0.,1.));
#8706=DIRECTION('center_axis',(-1.,0.,0.));
#8707=DIRECTION('ref_axis',(0.,0.,1.));
#8708=DIRECTION('center_axis',(-1.,0.,0.));
#8709=DIRECTION('ref_axis',(0.,0.,1.));
#8710=DIRECTION('center_axis',(1.,0.,0.));
#8711=DIRECTION('ref_axis',(0.,0.,-1.));
#8712=DIRECTION('center_axis',(1.,0.,0.));
#8713=DIRECTION('ref_axis',(0.,0.,-1.));
#8714=DIRECTION('center_axis',(0.,0.,-1.));
#8715=DIRECTION('ref_axis',(-1.,0.,0.));
#8716=DIRECTION('center_axis',(1.,0.,0.));
#8717=DIRECTION('ref_axis',(0.,0.,-1.));
#8718=DIRECTION('',(1.,0.,0.));
#8719=DIRECTION('center_axis',(1.,0.,0.));
#8720=DIRECTION('ref_axis',(0.,0.,-1.));
#8721=DIRECTION('',(1.,0.,0.));
#8722=DIRECTION('center_axis',(-1.,0.,0.));
#8723=DIRECTION('ref_axis',(0.,0.,1.));
#8724=DIRECTION('',(-1.,0.,0.));
#8725=DIRECTION('center_axis',(-1.,0.,0.));
#8726=DIRECTION('ref_axis',(0.,0.,1.));
#8727=DIRECTION('',(-1.,0.,0.));
#8728=DIRECTION('center_axis',(-1.,0.,0.));
#8729=DIRECTION('ref_axis',(0.,0.,1.));
#8730=DIRECTION('',(-1.,0.,0.));
#8731=DIRECTION('center_axis',(-1.,0.,0.));
#8732=DIRECTION('ref_axis',(0.,0.,1.));
#8733=DIRECTION('',(-1.,0.,0.));
#8734=DIRECTION('center_axis',(1.,0.,0.));
#8735=DIRECTION('ref_axis',(0.,0.,-1.));
#8736=DIRECTION('',(1.,0.,0.));
#8737=DIRECTION('center_axis',(1.,0.,0.));
#8738=DIRECTION('ref_axis',(0.,0.,-1.));
#8739=DIRECTION('',(1.,0.,0.));
#8740=DIRECTION('center_axis',(1.,0.,0.));
#8741=DIRECTION('ref_axis',(0.,0.,-1.));
#8742=DIRECTION('',(1.,0.,0.));
#8743=DIRECTION('axis',(0.,0.,1.));
#8744=DIRECTION('refdir',(1.,0.,0.));
#8745=DIRECTION('center_axis',(-1.,0.,0.));
#8746=DIRECTION('ref_axis',(0.,0.,1.));
#8747=DIRECTION('center_axis',(-1.,0.,0.));
#8748=DIRECTION('ref_axis',(0.,0.,1.));
#8749=DIRECTION('',(1.,0.,0.));
#8750=DIRECTION('center_axis',(-1.,0.,0.));
#8751=DIRECTION('ref_axis',(0.,0.,1.));
#8752=DIRECTION('center_axis',(1.,0.,0.));
#8753=DIRECTION('ref_axis',(0.,0.,-1.));
#8754=DIRECTION('center_axis',(1.,2.02536400451272E-15,-2.2981616621275E-15));
#8755=DIRECTION('ref_axis',(-2.2981616621275E-15,0.,-1.));
#8756=DIRECTION('center_axis',(-1.,0.,0.));
#8757=DIRECTION('ref_axis',(0.,0.,1.));
#8758=DIRECTION('center_axis',(-1.,0.,0.));
#8759=DIRECTION('ref_axis',(0.,0.,1.));
#8760=DIRECTION('center_axis',(-1.,0.,0.));
#8761=DIRECTION('ref_axis',(0.,0.,1.));
#8762=DIRECTION('',(1.,0.,0.));
#8763=DIRECTION('center_axis',(1.,-2.02536400451272E-15,2.2981616621275E-15));
#8764=DIRECTION('ref_axis',(2.2981616621275E-15,0.,-1.));
#8765=DIRECTION('center_axis',(-1.,0.,0.));
#8766=DIRECTION('ref_axis',(0.,0.,1.));
#8767=DIRECTION('center_axis',(-1.,0.,0.));
#8768=DIRECTION('ref_axis',(0.,0.,1.));
#8769=DIRECTION('center_axis',(-1.,0.,0.));
#8770=DIRECTION('ref_axis',(0.,0.,1.));
#8771=DIRECTION('',(1.,0.,0.));
#8772=DIRECTION('center_axis',(1.,0.,0.));
#8773=DIRECTION('ref_axis',(0.,0.,-1.));
#8774=DIRECTION('axis',(0.,0.,1.));
#8775=DIRECTION('refdir',(1.,0.,0.));
#8776=DIRECTION('axis',(0.,0.,1.));
#8777=DIRECTION('refdir',(1.,0.,0.));
#8778=DIRECTION('center_axis',(-1.,0.,0.));
#8779=DIRECTION('ref_axis',(0.,0.,1.));
#8780=DIRECTION('center_axis',(-1.,0.,0.));
#8781=DIRECTION('ref_axis',(0.,0.,1.));
#8782=DIRECTION('',(-1.,0.,0.));
#8783=DIRECTION('center_axis',(-1.,0.,0.));
#8784=DIRECTION('ref_axis',(0.,0.,1.));
#8785=DIRECTION('center_axis',(1.,-3.89528313553954E-16,9.13571080043379E-16));
#8786=DIRECTION('ref_axis',(9.13571080043379E-16,0.,-1.));
#8787=DIRECTION('',(0.,-0.49999998104077,0.866025414730555));
#8788=DIRECTION('',(-5.68434220074081E-15,-0.866025412838334,-0.499999984318193));
#8789=DIRECTION('center_axis',(-1.,0.,0.));
#8790=DIRECTION('ref_axis',(0.,0.,1.));
#8791=DIRECTION('',(0.,0.866025392838327,0.500000018959221));
#8792=DIRECTION('center_axis',(-1.,0.,0.));
#8793=DIRECTION('ref_axis',(0.,0.,1.));
#8794=DIRECTION('center_axis',(-1.,0.,0.));
#8795=DIRECTION('ref_axis',(0.,0.,1.));
#8796=DIRECTION('',(-1.,0.,0.));
#8797=DIRECTION('center_axis',(-1.,0.,0.));
#8798=DIRECTION('ref_axis',(0.,0.,1.));
#8799=DIRECTION('center_axis',(-3.98103628970969E-15,-0.500000018959218,
0.866025392838329));
#8800=DIRECTION('ref_axis',(3.30635451599776E-31,-0.866025392838329,-0.500000018959218));
#8801=DIRECTION('',(1.,0.,0.));
#8802=DIRECTION('',(0.,-0.866025392838343,-0.500000018959194));
#8803=DIRECTION('',(-1.,0.,0.));
#8804=DIRECTION('center_axis',(-1.,0.,0.));
#8805=DIRECTION('ref_axis',(0.,-0.866025406570393,-0.499999995174586));
#8806=DIRECTION('',(1.,0.,0.));
#8807=DIRECTION('center_axis',(-1.,0.,0.));
#8808=DIRECTION('ref_axis',(0.,0.,1.));
#8809=DIRECTION('center_axis',(1.04094622668064E-14,0.499999984318195,-0.866025412838333));
#8810=DIRECTION('ref_axis',(-1.37040070007528E-32,0.866025412838333,0.499999984318195));
#8811=DIRECTION('',(1.,0.,0.));
#8812=DIRECTION('',(0.,0.866025412838317,0.499999984318223));
#8813=DIRECTION('center_axis',(6.39983061249698E-15,-0.866025414730554,
-0.499999981040772));
#8814=DIRECTION('ref_axis',(4.36001107502503E-32,0.499999981040772,-0.866025414730554));
#8815=DIRECTION('',(0.,0.499999981040781,-0.866025414730549));
#8816=DIRECTION('center_axis',(1.,7.46138741516663E-16,2.73067399561958E-16));
#8817=DIRECTION('ref_axis',(-7.46138741516663E-16,1.,-2.54006882631165E-48));
#8818=DIRECTION('axis',(0.,0.,1.));
#8819=DIRECTION('refdir',(1.,0.,0.));
#8820=DIRECTION('center_axis',(0.,0.,-1.));
#8821=DIRECTION('ref_axis',(-1.,0.,0.));
#8822=DIRECTION('',(0.,1.,0.));
#8823=DIRECTION('',(-1.,0.,0.));
#8824=DIRECTION('',(0.,-1.,0.));
#8825=DIRECTION('',(1.,0.,0.));
#8826=DIRECTION('center_axis',(-7.28280409740021E-18,1.,-6.81994143705154E-16));
#8827=DIRECTION('ref_axis',(-2.00053299278642E-49,6.81994143705154E-16,
1.));
#8828=DIRECTION('',(0.,0.,1.));
#8829=DIRECTION('',(-1.,0.,0.));
#8830=DIRECTION('',(0.,0.,-1.));
#8831=DIRECTION('center_axis',(-1.,-9.93231300437194E-17,-1.29261680723712E-15));
#8832=DIRECTION('ref_axis',(-1.29261680723712E-15,0.,1.));
#8833=DIRECTION('',(0.,-1.,0.));
#8834=DIRECTION('',(0.,-0.107473383594446,-0.994207962057618));
#8835=DIRECTION('center_axis',(-1.,9.93231300437194E-17,1.29261680723712E-15));
#8836=DIRECTION('ref_axis',(1.29261680723712E-15,0.,1.));
#8837=DIRECTION('',(0.,-0.107473383594446,-0.994207962057618));
#8838=DIRECTION('',(0.,-1.,0.));
#8839=DIRECTION('center_axis',(-2.10796718596837E-17,-1.82172040081484E-16,
1.));
#8840=DIRECTION('ref_axis',(0.,-1.,-1.82172040081484E-16));
#8841=DIRECTION('',(-1.,0.,0.));
#8842=DIRECTION('center_axis',(5.30402919874122E-18,-0.994207962057617,
0.107473383594448));
#8843=DIRECTION('ref_axis',(1.08940721566226E-34,-0.107473383594448,-0.994207962057617));
#8844=DIRECTION('axis',(0.,0.,1.));
#8845=DIRECTION('refdir',(1.,0.,0.));
#8846=DIRECTION('center_axis',(1.,0.,0.));
#8847=DIRECTION('ref_axis',(0.,0.,-1.));
#8848=DIRECTION('center_axis',(1.,0.,0.));
#8849=DIRECTION('ref_axis',(0.,0.,-1.));
#8850=DIRECTION('',(1.,0.,0.));
#8851=DIRECTION('center_axis',(1.,0.,0.));
#8852=DIRECTION('ref_axis',(0.,0.,-1.));
#8853=DIRECTION('center_axis',(-1.,3.89528313543134E-16,9.13571080051068E-16));
#8854=DIRECTION('ref_axis',(9.13571080051068E-16,0.,1.));
#8855=DIRECTION('',(0.,0.499999981040771,-0.866025414730555));
#8856=DIRECTION('',(0.,-0.866025392838329,-0.500000018959218));
#8857=DIRECTION('center_axis',(1.,0.,0.));
#8858=DIRECTION('ref_axis',(0.,0.,-1.));
#8859=DIRECTION('',(1.1368683753664E-14,0.866025412838334,0.499999984318194));
#8860=DIRECTION('center_axis',(1.,0.,0.));
#8861=DIRECTION('ref_axis',(0.,0.,-1.));
#8862=DIRECTION('center_axis',(1.,0.,0.));
#8863=DIRECTION('ref_axis',(0.,0.,-1.));
#8864=DIRECTION('',(1.,0.,0.));
#8865=DIRECTION('center_axis',(1.,0.,0.));
#8866=DIRECTION('ref_axis',(0.,0.,-1.));
#8867=DIRECTION('center_axis',(1.0385048021943E-14,0.499999984318195,-0.866025412838333));
#8868=DIRECTION('ref_axis',(-5.27128262282187E-31,0.866025412838333,0.499999984318195));
#8869=DIRECTION('',(-1.,0.,0.));
#8870=DIRECTION('',(0.,-0.866025412838314,-0.499999984318228));
#8871=DIRECTION('',(1.,0.,0.));
#8872=DIRECTION('center_axis',(1.,0.,0.));
#8873=DIRECTION('ref_axis',(0.,0.,-1.));
#8874=DIRECTION('',(-1.,0.,0.));
#8875=DIRECTION('center_axis',(1.,0.,0.));
#8876=DIRECTION('ref_axis',(0.,0.,-1.));
#8877=DIRECTION('center_axis',(-3.97614054718644E-15,-0.500000018959218,
0.866025392838329));
#8878=DIRECTION('ref_axis',(3.1172350974474E-31,-0.866025392838329,-0.500000018959218));
#8879=DIRECTION('',(-1.,0.,0.));
#8880=DIRECTION('',(0.,0.866025392838324,0.500000018959226));
#8881=DIRECTION('center_axis',(6.40929678096138E-15,-0.866025414730554,
-0.499999981040772));
#8882=DIRECTION('ref_axis',(-1.92466517757951E-31,0.499999981040772,-0.866025414730554));
#8883=DIRECTION('',(0.,-0.499999981040781,0.866025414730549));
#8884=DIRECTION('center_axis',(-1.,-7.461387415107E-16,2.73067399557772E-16));
#8885=DIRECTION('ref_axis',(7.461387415107E-16,-1.,9.62450997316976E-49));
#8886=DIRECTION('axis',(0.,0.,1.));
#8887=DIRECTION('refdir',(1.,0.,0.));
#8888=DIRECTION('center_axis',(1.,0.,0.));
#8889=DIRECTION('ref_axis',(0.,0.,-1.));
#8890=DIRECTION('center_axis',(1.,0.,0.));
#8891=DIRECTION('ref_axis',(0.,0.,-1.));
#8892=DIRECTION('',(1.,0.,0.));
#8893=DIRECTION('center_axis',(1.,0.,0.));
#8894=DIRECTION('ref_axis',(0.,0.,-1.));
#8895=DIRECTION('center_axis',(-1.,-3.44325444684946E-17,-2.70173859336735E-18));
#8896=DIRECTION('ref_axis',(3.44325444684946E-17,-1.,-2.77218243538616E-51));
#8897=DIRECTION('',(0.,0.866025402838329,0.50000000163871));
#8898=DIRECTION('',(0.,-0.499999999594076,0.866025404018799));
#8899=DIRECTION('',(0.,0.107473447068807,0.994207955196069));
#8900=DIRECTION('',(0.,-0.994207960742926,0.107473395756311));
#8901=DIRECTION('',(0.,-0.107473446602436,-0.994207955246483));
#8902=DIRECTION('',(0.,0.499999999523326,-0.866025404059647));
#8903=DIRECTION('center_axis',(1.,0.,9.33194999941347E-14));
#8904=DIRECTION('ref_axis',(9.33194999941347E-14,0.,-1.));
#8905=DIRECTION('center_axis',(1.,0.,9.33194999941347E-14));
#8906=DIRECTION('ref_axis',(9.33194999941347E-14,0.,-1.));
#8907=DIRECTION('center_axis',(2.32889998828464E-18,0.866025404018799,0.499999999594076));
#8908=DIRECTION('ref_axis',(-1.13747398687096E-34,-0.499999999594076,0.866025404018799));
#8909=DIRECTION('',(1.,0.,0.));
#8910=DIRECTION('',(0.,0.499999999594074,-0.8660254040188));
#8911=DIRECTION('',(1.,0.,0.));
#8912=DIRECTION('',(0.,-0.499999999594075,0.866025404018799));
#8913=DIRECTION('',(-1.,0.,0.));
#8914=DIRECTION('',(1.,0.,0.));
#8915=DIRECTION('',(0.,-0.499999999594074,0.8660254040188));
#8916=DIRECTION('center_axis',(-2.99047289596199E-18,0.994207955196069,
-0.107473447068807));
#8917=DIRECTION('ref_axis',(1.7192384968967E-36,0.107473447068807,0.994207955196069));
#8918=DIRECTION('',(0.,0.107473447068808,0.994207955196069));
#8919=DIRECTION('',(-1.,0.,0.));
#8920=DIRECTION('center_axis',(-3.44011407178642E-19,0.10747339575632,0.994207960742925));
#8921=DIRECTION('ref_axis',(-9.20601768266839E-37,-0.994207960742925,0.10747339575632));
#8922=DIRECTION('',(0.,-0.994207960742924,0.107473395756334));
#8923=DIRECTION('',(-1.,0.,0.));
#8924=DIRECTION('center_axis',(1.21066295142474E-17,-0.994207955246483,
0.107473446602436));
#8925=DIRECTION('ref_axis',(-1.21784695446604E-33,-0.107473446602436,-0.994207955246483));
#8926=DIRECTION('',(0.,-0.107473446602435,-0.994207955246483));
#8927=DIRECTION('',(-1.,0.,0.));
#8928=DIRECTION('center_axis',(2.27934427627508E-17,-0.866025404059647,
-0.499999999523326));
#8929=DIRECTION('ref_axis',(9.40315152180257E-34,0.499999999523326,-0.866025404059647));
#8930=DIRECTION('',(-1.,0.,0.));
#8931=DIRECTION('',(0.,-0.499999999523324,0.866025404059648));
#8932=DIRECTION('',(-1.,0.,0.));
#8933=DIRECTION('',(0.,0.499999999523324,-0.866025404059648));
#8934=DIRECTION('',(-1.,0.,0.));
#8935=DIRECTION('',(0.,0.499999999523327,-0.866025404059646));
#8936=DIRECTION('center_axis',(1.,-3.36352380295954E-15,-3.1884171780454E-16));
#8937=DIRECTION('ref_axis',(3.36352380295954E-15,1.,-1.57533431125151E-47));
#8938=DIRECTION('',(0.,-0.866025402838331,-0.500000001638706));
#8939=DIRECTION('',(0.,1.,0.));
#8940=DIRECTION('center_axis',(1.,0.,0.));
#8941=DIRECTION('ref_axis',(0.,0.,-1.));
#8942=DIRECTION('center_axis',(1.86029643864781E-15,0.500000001638701,-0.866025402838334));
#8943=DIRECTION('ref_axis',(-2.70969563331381E-32,0.866025402838334,0.500000001638701));
#8944=DIRECTION('',(0.,0.866025402838314,0.500000001638735));
#8945=DIRECTION('center_axis',(-1.,3.44325444684946E-17,2.70173859336735E-18));
#8946=DIRECTION('ref_axis',(-3.44325444684946E-17,-1.,-2.77218243538616E-51));
#8947=DIRECTION('center_axis',(1.,0.,0.));
#8948=DIRECTION('ref_axis',(0.,0.,-1.));
#8949=DIRECTION('center_axis',(1.86511836885772E-15,0.500000001638701,-0.866025402838334));
#8950=DIRECTION('ref_axis',(-6.80058163600059E-32,0.866025402838334,0.500000001638701));
#8951=DIRECTION('',(0.,0.866025402838379,0.500000001638623));
#8952=DIRECTION('center_axis',(1.,3.36352380295954E-15,3.1884171780454E-16));
#8953=DIRECTION('ref_axis',(-3.36352380295954E-15,1.,-1.57533431125151E-47));
#8954=DIRECTION('',(0.,1.,0.));
#8955=DIRECTION('center_axis',(1.,0.,9.33194999941347E-14));
#8956=DIRECTION('ref_axis',(9.33194999941347E-14,0.,-1.));
#8957=DIRECTION('center_axis',(1.,0.,9.33194999941347E-14));
#8958=DIRECTION('ref_axis',(9.33194999941347E-14,0.,-1.));
#8959=DIRECTION('center_axis',(-1.82558994376595E-17,5.45297246983656E-15,
-1.));
#8960=DIRECTION('ref_axis',(0.,1.,5.45297246983656E-15));
#8961=DIRECTION('center_axis',(1.,0.,9.33194999941347E-14));
#8962=DIRECTION('ref_axis',(9.33194999941347E-14,0.,-1.));
#8963=DIRECTION('',(1.,0.,9.33194999941347E-14));
#8964=DIRECTION('center_axis',(1.,0.,9.33194999941347E-14));
#8965=DIRECTION('ref_axis',(9.33194999941347E-14,0.,-1.));
#8966=DIRECTION('',(1.,0.,9.33194999941347E-14));
#8967=DIRECTION('center_axis',(1.,0.,0.));
#8968=DIRECTION('ref_axis',(0.,0.,-1.));
#8969=DIRECTION('',(1.,0.,0.));
#8970=DIRECTION('axis',(0.,0.,1.));
#8971=DIRECTION('refdir',(1.,0.,0.));
#8972=DIRECTION('center_axis',(1.,0.,0.));
#8973=DIRECTION('ref_axis',(0.,0.,-1.));
#8974=DIRECTION('center_axis',(1.,0.,0.));
#8975=DIRECTION('ref_axis',(0.,0.,-1.));
#8976=DIRECTION('',(1.,0.,0.));
#8977=DIRECTION('center_axis',(1.,0.,0.));
#8978=DIRECTION('ref_axis',(0.,0.,-1.));
#8979=DIRECTION('center_axis',(-1.,4.48048999173929E-16,8.23217897594901E-17));
#8980=DIRECTION('ref_axis',(-4.48048999173929E-16,-1.,-9.21527566961904E-49));
#8981=DIRECTION('',(4.92278448714275E-15,0.499999981040771,-0.866025414730555));
#8982=DIRECTION('',(0.,-0.866025392838329,-0.500000018959218));
#8983=DIRECTION('center_axis',(1.,0.,0.));
#8984=DIRECTION('ref_axis',(0.,0.,-1.));
#8985=DIRECTION('',(0.,0.866025412838334,0.499999984318194));
#8986=DIRECTION('center_axis',(1.,0.,0.));
#8987=DIRECTION('ref_axis',(0.,0.,-1.));
#8988=DIRECTION('center_axis',(1.,0.,0.));
#8989=DIRECTION('ref_axis',(0.,0.,-1.));
#8990=DIRECTION('',(1.,0.,0.));
#8991=DIRECTION('center_axis',(1.,0.,0.));
#8992=DIRECTION('ref_axis',(0.,0.,-1.));
#8993=DIRECTION('center_axis',(1.02825143608802E-14,0.499999984318195,-0.866025412838333));
#8994=DIRECTION('ref_axis',(1.50357456271857E-31,0.866025412838333,0.499999984318195));
#8995=DIRECTION('',(-1.,0.,0.));
#8996=DIRECTION('',(0.,-0.866025412838314,-0.499999984318228));
#8997=DIRECTION('',(1.,0.,0.));
#8998=DIRECTION('center_axis',(1.,0.,0.));
#8999=DIRECTION('ref_axis',(0.,0.,-1.));
#9000=DIRECTION('',(-1.,0.,0.));
#9001=DIRECTION('center_axis',(1.,0.,0.));
#9002=DIRECTION('ref_axis',(0.,0.,-1.));
#9003=DIRECTION('center_axis',(-4.00530144163786E-15,-0.500000018959218,
0.866025392838329));
#9004=DIRECTION('ref_axis',(1.5507230852345E-31,-0.866025392838329,-0.500000018959218));
#9005=DIRECTION('',(-1.,0.,0.));
#9006=DIRECTION('',(0.,0.866025392838324,0.500000018959226));
#9007=DIRECTION('center_axis',(6.45242124694183E-15,-0.866025414730554,
-0.499999981040772));
#9008=DIRECTION('ref_axis',(1.49042295424067E-31,0.499999981040772,-0.866025414730554));
#9009=DIRECTION('',(0.,-0.499999981040781,0.866025414730549));
#9010=DIRECTION('center_axis',(-1.,-4.77309341971722E-16,2.03395055774814E-15));
#9011=DIRECTION('ref_axis',(2.03395055774814E-15,0.,1.));
#9012=DIRECTION('axis',(0.,0.,1.));
#9013=DIRECTION('refdir',(1.,0.,0.));
#9014=DIRECTION('center_axis',(-1.,0.,0.));
#9015=DIRECTION('ref_axis',(0.,0.,1.));
#9016=DIRECTION('center_axis',(-1.,0.,0.));
#9017=DIRECTION('ref_axis',(0.,0.,1.));
#9018=DIRECTION('',(-1.,0.,0.));
#9019=DIRECTION('center_axis',(-1.,0.,0.));
#9020=DIRECTION('ref_axis',(0.,0.,1.));
#9021=DIRECTION('center_axis',(1.,-4.4804899918026E-16,8.23217897544922E-17));
#9022=DIRECTION('ref_axis',(4.4804899918026E-16,1.,2.26725874505889E-48));
#9023=DIRECTION('',(0.,-0.49999998104077,0.866025414730555));
#9024=DIRECTION('',(5.68434220074081E-15,-0.866025412838334,-0.499999984318193));
#9025=DIRECTION('center_axis',(-1.,0.,0.));
#9026=DIRECTION('ref_axis',(0.,0.,1.));
#9027=DIRECTION('',(0.,0.866025392838327,0.500000018959221));
#9028=DIRECTION('center_axis',(-1.,0.,0.));
#9029=DIRECTION('ref_axis',(0.,0.,1.));
#9030=DIRECTION('center_axis',(-1.,0.,0.));
#9031=DIRECTION('ref_axis',(0.,0.,1.));
#9032=DIRECTION('',(-1.,0.,0.));
#9033=DIRECTION('center_axis',(-1.,0.,0.));
#9034=DIRECTION('ref_axis',(0.,0.,1.));
#9035=DIRECTION('center_axis',(-3.99107463157378E-15,-0.500000018959218,
0.866025392838329));
#9036=DIRECTION('ref_axis',(7.48434538625964E-32,-0.866025392838329,-0.500000018959218));
#9037=DIRECTION('',(1.,0.,0.));
#9038=DIRECTION('',(0.,-0.866025392838343,-0.500000018959194));
#9039=DIRECTION('',(-1.,0.,0.));
#9040=DIRECTION('center_axis',(-1.,0.,0.));
#9041=DIRECTION('ref_axis',(0.,-0.866025406570393,-0.499999995174586));
#9042=DIRECTION('',(1.,0.,0.));
#9043=DIRECTION('center_axis',(-1.,0.,0.));
#9044=DIRECTION('ref_axis',(0.,0.,1.));
#9045=DIRECTION('center_axis',(1.04209967862532E-14,0.499999984318195,-0.866025412838333));
#9046=DIRECTION('ref_axis',(4.87803011688087E-32,0.866025412838333,0.499999984318195));
#9047=DIRECTION('',(1.,0.,0.));
#9048=DIRECTION('',(0.,0.866025412838317,0.499999984318223));
#9049=DIRECTION('center_axis',(6.43478340347328E-15,-0.866025414730554,
-0.499999981040772));
#9050=DIRECTION('ref_axis',(6.55419316660567E-32,0.499999981040772,-0.866025414730554));
#9051=DIRECTION('',(0.,0.499999981040781,-0.866025414730549));
#9052=DIRECTION('center_axis',(1.,1.49593502589698E-15,6.8668419608312E-16));
#9053=DIRECTION('ref_axis',(-1.49593502589698E-15,1.,8.50544090484151E-47));
#9054=DIRECTION('',(0.,0.,1.));
#9055=DIRECTION('',(1.,0.,0.));
#9056=DIRECTION('',(0.,0.,1.));
#9057=DIRECTION('',(1.,0.,0.));
#9058=DIRECTION('',(0.,0.,1.));
#9059=DIRECTION('',(1.,0.,0.));
#9060=DIRECTION('',(0.,0.,1.));
#9061=DIRECTION('',(1.,0.,0.));
#9062=DIRECTION('',(0.,0.,1.));
#9063=DIRECTION('',(1.,0.,0.));
#9064=DIRECTION('',(0.,0.,1.));
#9065=DIRECTION('',(1.,0.,0.));
#9066=DIRECTION('axis',(0.,0.,1.));
#9067=DIRECTION('refdir',(1.,0.,0.));
#9068=DIRECTION('axis',(0.,0.,1.));
#9069=DIRECTION('refdir',(1.,0.,0.));
#9070=DIRECTION('center_axis',(1.,0.,2.22044604925031E-15));
#9071=DIRECTION('ref_axis',(2.22044604925031E-15,0.,-1.));
#9072=DIRECTION('center_axis',(0.707106781186548,0.530215432236494,-0.467837146257399));
#9073=DIRECTION('ref_axis',(0.707106781186547,-0.530215432236493,0.467837146257402));
#9074=DIRECTION('center_axis',(0.707106781186547,-0.530215432236493,0.467837146257402));
#9075=DIRECTION('ref_axis',(0.707106781186548,0.530215432236494,-0.467837146257399));
#9076=DIRECTION('center_axis',(0.,-0.749837855248362,0.661621637219141));
#9077=DIRECTION('ref_axis',(0.,-0.661621637219141,-0.749837855248362));
#9078=DIRECTION('',(0.,0.749837855248362,-0.661621637219141));
#9079=DIRECTION('center_axis',(-0.707106781186548,0.530215432236494,-0.4678371462574));
#9080=DIRECTION('ref_axis',(-0.707106781186547,-0.530215432236494,0.4678371462574));
#9081=DIRECTION('center_axis',(-0.707106781186548,-0.530215432236494,0.4678371462574));
#9082=DIRECTION('ref_axis',(-0.707106781186547,0.530215432236494,-0.4678371462574));
#9083=DIRECTION('center_axis',(-1.,0.,0.));
#9084=DIRECTION('ref_axis',(0.,0.,1.));
#9085=DIRECTION('axis',(0.,0.,1.));
#9086=DIRECTION('refdir',(1.,0.,0.));
#9087=DIRECTION('center_axis',(1.,0.,0.));
#9088=DIRECTION('ref_axis',(0.,0.,-1.));
#9089=DIRECTION('center_axis',(1.,0.,0.));
#9090=DIRECTION('ref_axis',(0.,0.,-1.));
#9091=DIRECTION('',(-1.,0.,0.));
#9092=DIRECTION('center_axis',(1.,0.,0.));
#9093=DIRECTION('ref_axis',(0.,0.,-1.));
#9094=DIRECTION('center_axis',(-1.,2.37904933965006E-16,7.4543545972162E-17));
#9095=DIRECTION('ref_axis',(-2.37904933965006E-16,-1.,1.16006348247081E-48));
#9096=DIRECTION('center_axis',(-1.,-2.37904933965006E-16,-7.4543545972162E-17));
#9097=DIRECTION('ref_axis',(2.37904933965006E-16,-1.,1.16006348247081E-48));
#9098=DIRECTION('axis',(0.,0.,1.));
#9099=DIRECTION('refdir',(1.,0.,0.));
#9100=DIRECTION('center_axis',(-1.,0.,0.));
#9101=DIRECTION('ref_axis',(0.,0.,1.));
#9102=DIRECTION('center_axis',(-1.,0.,0.));
#9103=DIRECTION('ref_axis',(0.,0.,1.));
#9104=DIRECTION('',(-1.,0.,0.));
#9105=DIRECTION('center_axis',(-1.,0.,0.));
#9106=DIRECTION('ref_axis',(0.,0.,1.));
#9107=DIRECTION('center_axis',(1.,0.,0.));
#9108=DIRECTION('ref_axis',(0.,0.,-1.));
#9109=DIRECTION('center_axis',(-1.,0.,0.));
#9110=DIRECTION('ref_axis',(0.,0.,1.));
#9111=DIRECTION('center_axis',(1.,0.,0.));
#9112=DIRECTION('ref_axis',(0.,0.,-1.));
#9113=DIRECTION('center_axis',(-1.,0.,0.));
#9114=DIRECTION('ref_axis',(0.,0.,1.));
#9115=DIRECTION('center_axis',(-1.,0.,0.));
#9116=DIRECTION('ref_axis',(0.,0.,1.));
#9117=DIRECTION('',(1.,0.,0.));
#9118=DIRECTION('axis',(0.,0.,1.));
#9119=DIRECTION('refdir',(1.,0.,0.));
#9120=DIRECTION('center_axis',(-1.,0.,2.22044604925031E-15));
#9121=DIRECTION('ref_axis',(-1.46909515046131E-15,0.749837855248542,-0.661621637218937));
#9122=DIRECTION('center_axis',(-0.707106781186548,0.530215432236494,-0.467837146257399));
#9123=DIRECTION('ref_axis',(-0.707106781186547,-0.530215432236493,0.467837146257402));
#9124=DIRECTION('center_axis',(-0.707106781186547,-0.530215432236493,0.467837146257402));
#9125=DIRECTION('ref_axis',(-0.707106781186548,0.530215432236494,-0.467837146257399));
#9126=DIRECTION('center_axis',(0.,-0.749837855248362,0.661621637219141));
#9127=DIRECTION('ref_axis',(0.,-0.661621637219141,-0.749837855248362));
#9128=DIRECTION('',(0.,0.749837855248362,-0.661621637219141));
#9129=DIRECTION('center_axis',(0.707106781186548,-0.530215432236494,0.4678371462574));
#9130=DIRECTION('ref_axis',(0.707106781186547,0.530215432236494,-0.4678371462574));
#9131=DIRECTION('center_axis',(0.707106781186548,0.530215432236494,-0.4678371462574));
#9132=DIRECTION('ref_axis',(0.707106781186547,-0.530215432236494,0.4678371462574));
#9133=DIRECTION('center_axis',(1.,0.,0.));
#9134=DIRECTION('ref_axis',(0.,-0.74983785524939,0.661621637217976));
#9135=DIRECTION('axis',(0.,0.,1.));
#9136=DIRECTION('refdir',(1.,0.,0.));
#9137=DIRECTION('center_axis',(-1.,0.,0.));
#9138=DIRECTION('ref_axis',(0.,0.,1.));
#9139=DIRECTION('center_axis',(-1.,0.,0.));
#9140=DIRECTION('ref_axis',(0.,0.,1.));
#9141=DIRECTION('',(1.,0.,0.));
#9142=DIRECTION('center_axis',(-1.,0.,0.));
#9143=DIRECTION('ref_axis',(0.,0.,1.));
#9144=DIRECTION('center_axis',(1.,1.14194368292889E-16,-1.4591502616446E-16));
#9145=DIRECTION('ref_axis',(-1.4591502616446E-16,0.,-1.));
#9146=DIRECTION('center_axis',(1.,-1.14194368292889E-16,1.4591502616446E-16));
#9147=DIRECTION('ref_axis',(1.4591502616446E-16,0.,-1.));
#9148=DIRECTION('',(0.,0.,1.));
#9149=DIRECTION('',(1.,0.,0.));
#9150=DIRECTION('',(0.,0.,1.));
#9151=DIRECTION('',(1.,0.,0.));
#9152=DIRECTION('',(0.,0.,1.));
#9153=DIRECTION('',(1.,0.,0.));
#9154=DIRECTION('',(0.,0.,1.));
#9155=DIRECTION('',(1.,0.,0.));
#9156=DIRECTION('',(0.,0.,1.));
#9157=DIRECTION('',(1.,0.,0.));
#9158=DIRECTION('axis',(0.,0.,1.));
#9159=DIRECTION('refdir',(1.,0.,0.));
#9160=DIRECTION('center_axis',(-1.,0.,0.));
#9161=DIRECTION('ref_axis',(0.,0.,1.));
#9162=DIRECTION('center_axis',(-1.,0.,0.));
#9163=DIRECTION('ref_axis',(0.,0.,1.));
#9164=DIRECTION('',(1.,0.,0.));
#9165=DIRECTION('center_axis',(-1.,0.,0.));
#9166=DIRECTION('ref_axis',(0.,0.,1.));
#9167=DIRECTION('center_axis',(1.,-9.9268665898833E-16,1.01959257413342E-15));
#9168=DIRECTION('ref_axis',(1.01959257413342E-15,0.,-1.));
#9169=DIRECTION('center_axis',(1.,0.,0.));
#9170=DIRECTION('ref_axis',(0.,0.,-1.));
#9171=DIRECTION('center_axis',(-1.,0.,0.));
#9172=DIRECTION('ref_axis',(0.,0.,1.));
#9173=DIRECTION('',(0.,0.,1.));
#9174=DIRECTION('',(0.,-1.,1.98951966438983E-14));
#9175=DIRECTION('center_axis',(1.,0.,0.));
#9176=DIRECTION('ref_axis',(0.,0.,-1.));
#9177=DIRECTION('center_axis',(1.,0.,0.));
#9178=DIRECTION('ref_axis',(0.,0.,-1.));
#9179=DIRECTION('center_axis',(1.,0.,0.));
#9180=DIRECTION('ref_axis',(0.,0.,-1.));
#9181=DIRECTION('center_axis',(1.,0.,0.));
#9182=DIRECTION('ref_axis',(0.,0.,-1.));
#9183=DIRECTION('center_axis',(1.,0.,0.));
#9184=DIRECTION('ref_axis',(0.,0.,-1.));
#9185=DIRECTION('center_axis',(1.,0.,0.));
#9186=DIRECTION('ref_axis',(0.,0.,-1.));
#9187=DIRECTION('center_axis',(1.,0.,0.));
#9188=DIRECTION('ref_axis',(0.,0.,-1.));
#9189=DIRECTION('center_axis',(1.,0.,0.));
#9190=DIRECTION('ref_axis',(0.,0.,-1.));
#9191=DIRECTION('',(1.,0.,0.));
#9192=DIRECTION('center_axis',(1.,0.,0.));
#9193=DIRECTION('ref_axis',(0.,0.,-1.));
#9194=DIRECTION('center_axis',(1.,0.,0.));
#9195=DIRECTION('ref_axis',(0.,0.,-1.));
#9196=DIRECTION('',(1.,0.,0.));
#9197=DIRECTION('center_axis',(1.,0.,0.));
#9198=DIRECTION('ref_axis',(0.,0.,-1.));
#9199=DIRECTION('center_axis',(1.,0.,0.));
#9200=DIRECTION('ref_axis',(0.,0.,-1.));
#9201=DIRECTION('',(1.,0.,0.));
#9202=DIRECTION('center_axis',(1.,0.,0.));
#9203=DIRECTION('ref_axis',(0.,0.,-1.));
#9204=DIRECTION('center_axis',(1.,0.,0.));
#9205=DIRECTION('ref_axis',(0.,0.,-1.));
#9206=DIRECTION('',(1.,0.,0.));
#9207=DIRECTION('center_axis',(1.,0.,0.));
#9208=DIRECTION('ref_axis',(0.,0.,-1.));
#9209=DIRECTION('center_axis',(1.,0.,0.));
#9210=DIRECTION('ref_axis',(0.,0.,-1.));
#9211=DIRECTION('',(1.,0.,0.));
#9212=DIRECTION('center_axis',(2.20458572024499E-15,5.64627709665039E-16,
1.));
#9213=DIRECTION('ref_axis',(1.,5.1073991127734E-47,-2.20458572024499E-15));
#9214=DIRECTION('',(-1.,0.,0.));
#9215=DIRECTION('',(1.,0.,0.));
#9216=DIRECTION('',(0.,-1.,0.));
#9217=DIRECTION('center_axis',(1.,0.,0.));
#9218=DIRECTION('ref_axis',(0.,0.,-1.));
#9219=DIRECTION('center_axis',(1.,0.,0.));
#9220=DIRECTION('ref_axis',(0.,0.,-1.));
#9221=DIRECTION('',(1.,0.,0.));
#9222=DIRECTION('center_axis',(1.,0.,0.));
#9223=DIRECTION('ref_axis',(0.,0.267643864798619,0.963517909348684));
#9224=DIRECTION('',(-1.,0.,0.));
#9225=DIRECTION('center_axis',(1.,0.,0.));
#9226=DIRECTION('ref_axis',(0.,0.,-1.));
#9227=DIRECTION('center_axis',(3.68752646949032E-16,-1.,-1.69617406532146E-17));
#9228=DIRECTION('ref_axis',(1.,3.68752646949032E-16,0.));
#9229=DIRECTION('',(0.,0.,-1.));
#9230=DIRECTION('center_axis',(-1.,0.,0.));
#9231=DIRECTION('ref_axis',(0.,0.,1.));
#9232=DIRECTION('axis',(0.,0.,1.));
#9233=DIRECTION('refdir',(1.,0.,0.));
#9234=DIRECTION('axis',(0.,0.,1.));
#9235=DIRECTION('refdir',(1.,0.,0.));
#9236=DIRECTION('center_axis',(-1.,0.,0.));
#9237=DIRECTION('ref_axis',(0.,0.,1.));
#9238=DIRECTION('center_axis',(-1.,0.,0.));
#9239=DIRECTION('ref_axis',(0.,0.,1.));
#9240=DIRECTION('',(-1.,0.,0.));
#9241=DIRECTION('center_axis',(-1.,0.,0.));
#9242=DIRECTION('ref_axis',(0.,0.,1.));
#9243=DIRECTION('center_axis',(1.,4.89404439732965E-17,-4.89404438350122E-17));
#9244=DIRECTION('ref_axis',(-4.89404439732965E-17,1.,-7.23876700762992E-50));
#9245=DIRECTION('center_axis',(-1.,0.,0.));
#9246=DIRECTION('ref_axis',(0.,0.,1.));
#9247=DIRECTION('center_axis',(1.,0.,0.));
#9248=DIRECTION('ref_axis',(0.,0.,-1.));
#9249=DIRECTION('center_axis',(-1.,0.,0.));
#9250=DIRECTION('ref_axis',(0.,0.,1.));
#9251=DIRECTION('center_axis',(-1.,0.,0.));
#9252=DIRECTION('ref_axis',(0.,0.,1.));
#9253=DIRECTION('',(1.,0.,0.));
#9254=DIRECTION('axis',(0.,0.,1.));
#9255=DIRECTION('refdir',(1.,0.,0.));
#9256=DIRECTION('center_axis',(1.,0.,0.));
#9257=DIRECTION('ref_axis',(0.,0.,-1.));
#9258=DIRECTION('center_axis',(1.,0.,0.));
#9259=DIRECTION('ref_axis',(0.,0.,-1.));
#9260=DIRECTION('',(1.,0.,0.));
#9261=DIRECTION('center_axis',(1.,0.,0.));
#9262=DIRECTION('ref_axis',(0.,0.,-1.));
#9263=DIRECTION('center_axis',(-1.,-4.89404439732087E-17,-4.89404438350122E-17));
#9264=DIRECTION('ref_axis',(4.89404439732087E-17,-1.,5.74495806648814E-50));
#9265=DIRECTION('center_axis',(1.,0.,0.));
#9266=DIRECTION('ref_axis',(0.,0.,-1.));
#9267=DIRECTION('center_axis',(-1.,0.,0.));
#9268=DIRECTION('ref_axis',(0.,0.,1.));
#9269=DIRECTION('center_axis',(1.,0.,0.));
#9270=DIRECTION('ref_axis',(0.,0.,-1.));
#9271=DIRECTION('center_axis',(1.,0.,0.));
#9272=DIRECTION('ref_axis',(0.,0.,-1.));
#9273=DIRECTION('',(-1.,0.,0.));
#9274=DIRECTION('axis',(0.,0.,1.));
#9275=DIRECTION('refdir',(1.,0.,0.));
#9276=DIRECTION('center_axis',(-1.,0.,0.));
#9277=DIRECTION('ref_axis',(0.,0.,1.));
#9278=DIRECTION('center_axis',(-1.,0.,0.));
#9279=DIRECTION('ref_axis',(0.,0.,1.));
#9280=DIRECTION('',(1.,0.,0.));
#9281=DIRECTION('center_axis',(-1.,0.,0.));
#9282=DIRECTION('ref_axis',(0.,0.,1.));
#9283=DIRECTION('center_axis',(1.,-4.74223835053899E-16,3.88578058810774E-16));
#9284=DIRECTION('ref_axis',(4.74223835053899E-16,1.,-6.83343688678077E-48));
#9285=DIRECTION('center_axis',(1.,4.74223835053899E-16,-3.88578058810774E-16));
#9286=DIRECTION('ref_axis',(-4.74223835053899E-16,1.,-6.83343688678077E-48));
#9287=DIRECTION('',(0.,0.724095872437622,0.689699331244275));
#9288=DIRECTION('',(-1.,0.,0.));
#9289=DIRECTION('',(0.,0.724095872437622,0.689699331244275));
#9290=DIRECTION('',(-1.,0.,0.));
#9291=DIRECTION('',(0.,0.724095872437622,0.689699331244275));
#9292=DIRECTION('',(-1.,0.,0.));
#9293=DIRECTION('',(1.,0.,0.));
#9294=DIRECTION('',(0.,0.443359804928245,-0.896343730593341));
#9295=DIRECTION('',(0.,0.,1.));
#9296=DIRECTION('',(1.,0.,0.));
#9297=DIRECTION('',(0.,-0.0378713914675926,0.999282621538226));
#9298=DIRECTION('',(1.,0.,0.));
#9299=DIRECTION('',(1.,0.,0.));
#9300=DIRECTION('',(0.,0.178546941054999,-0.983931394884777));
#9301=DIRECTION('',(1.,0.,0.));
#9302=DIRECTION('',(0.,0.,-1.));
#9303=DIRECTION('',(0.,0.,1.));
#9304=DIRECTION('',(1.,0.,0.));
#9305=DIRECTION('',(0.,0.,1.));
#9306=DIRECTION('',(1.,0.,0.));
#9307=DIRECTION('',(0.,0.,-1.));
#9308=DIRECTION('',(-1.,0.,0.));
#9309=DIRECTION('',(0.,0.,1.));
#9310=DIRECTION('',(1.,0.,0.));
#9311=DIRECTION('',(0.,0.,1.));
#9312=DIRECTION('',(1.,0.,0.));
#9313=DIRECTION('',(0.,0.,1.));
#9314=DIRECTION('',(1.,0.,0.));
#9315=DIRECTION('',(0.,0.,1.));
#9316=DIRECTION('',(1.,0.,0.));
#9317=DIRECTION('',(0.,0.,1.));
#9318=DIRECTION('',(1.,0.,0.));
#9319=DIRECTION('',(0.,0.,1.));
#9320=DIRECTION('',(1.,0.,0.));
#9321=DIRECTION('',(0.,0.,1.));
#9322=DIRECTION('',(1.,0.,0.));
#9323=DIRECTION('',(0.,0.,1.));
#9324=DIRECTION('',(1.,0.,0.));
#9325=CARTESIAN_POINT('',(0.,0.,0.));
#9326=CARTESIAN_POINT('',(0.,0.,0.));
#9327=CARTESIAN_POINT('Origin',(5.92883964145585E-11,1.19863443615031E-10,
-0.0065));
#9328=CARTESIAN_POINT('',(-0.00749999969312043,1.09515285974588E-10,0.0065));
#9329=CARTESIAN_POINT('Origin',(5.92883964145585E-11,1.19863443615031E-10,
0.0065));
#9330=CARTESIAN_POINT('',(-0.00749999969312043,1.09515287811566E-10,-0.0065));
#9331=CARTESIAN_POINT('',(-0.00749999969312043,1.09515285974588E-10,-0.0065));
#9332=CARTESIAN_POINT('Origin',(5.92883964145585E-11,1.19863443615031E-10,
-0.0065));
#9333=CARTESIAN_POINT('Origin',(-5.74005956283549E-52,0.,0.015));
#9334=CARTESIAN_POINT('',(-0.042,-1.9853686361416E-11,0.007381198));
#9335=CARTESIAN_POINT('Origin',(-2.66453525910038E-17,5.09119415777057E-18,
0.007381198));
#9336=CARTESIAN_POINT('',(-0.042,-1.54820701770975E-11,-0.007381198));
#9337=CARTESIAN_POINT('',(-0.042,-5.14351655641888E-18,0.015));
#9338=CARTESIAN_POINT('',(0.0419999999999985,-5.1435165564187E-18,-0.00738119800000199));
#9339=CARTESIAN_POINT('Origin',(-8.88178419700125E-18,-5.73557577313579E-18,
-0.007381198));
#9340=CARTESIAN_POINT('Origin',(-8.88178419700125E-18,-5.73557577313579E-18,
-0.007381198));
#9341=CARTESIAN_POINT('Origin',(-2.64244881468667E-16,0.,-0.560482737499999));
#9342=CARTESIAN_POINT('',(0.0499999999999997,-6.12323399573673E-18,-0.0120000000000027));
#9343=CARTESIAN_POINT('Origin',(8.88178419700125E-18,1.23918456012259E-18,
-0.012000000000002));
#9344=CARTESIAN_POINT('',(1.,-1.22464679914735E-16,-0.5604827375));
#9345=CARTESIAN_POINT('Origin',(2.63459037944631E-16,0.,0.560482737500119));
#9346=CARTESIAN_POINT('',(0.05,-2.05102985990085E-11,0.0120000000000921));
#9347=CARTESIAN_POINT('',(-0.0499999999999868,-6.12323399573515E-18,0.0120000000001151));
#9348=CARTESIAN_POINT('Origin',(1.77635683940025E-17,-6.31136467490802E-18,
0.0120000000000921));
#9349=CARTESIAN_POINT('',(-1.,-1.22464679914735E-16,0.560482737500119));
#9350=CARTESIAN_POINT('Origin',(1.77635683940025E-17,-6.31136467490802E-18,
0.0120000000000921));
#9351=CARTESIAN_POINT('Origin',(0.,0.,0.015));
#9352=CARTESIAN_POINT('',(0.05,-6.12323399573677E-18,-0.015));
#9353=CARTESIAN_POINT('Origin',(0.,0.,-0.015));
#9354=CARTESIAN_POINT('',(0.05,-6.12323399573677E-18,0.015));
#9355=CARTESIAN_POINT('Origin',(0.,0.,0.015));
#9356=CARTESIAN_POINT('',(0.05,-6.12323399573677E-18,0.015));
#9357=CARTESIAN_POINT('',(0.05,-6.12323399573677E-18,0.015));
#9358=CARTESIAN_POINT('Origin',(0.,0.,0.015));
#9359=CARTESIAN_POINT('Origin',(5.79397640976254E-18,1.73472347597681E-19,
-0.015));
#9360=CARTESIAN_POINT('',(0.04,-4.89858719658941E-18,-0.015));
#9361=CARTESIAN_POINT('Origin',(-6.50521303491303E-19,0.,-0.015));
#9362=CARTESIAN_POINT('Origin',(5.79397640976254E-18,1.73472347597681E-19,
0.015));
#9363=CARTESIAN_POINT('',(0.04,-4.89858719658941E-18,0.015));
#9364=CARTESIAN_POINT('Origin',(0.,0.,0.015));
#9365=CARTESIAN_POINT('Origin',(1.85684700327654E-52,0.,0.015));
#9366=CARTESIAN_POINT('',(0.04,-4.89858719658941E-18,-0.005));
#9367=CARTESIAN_POINT('Origin',(-4.33680868994202E-19,0.,-0.005));
#9368=CARTESIAN_POINT('',(0.04,-4.89858719658941E-18,0.015));
#9369=CARTESIAN_POINT('Origin',(0.,0.,0.015));
#9370=CARTESIAN_POINT('',(0.04,-4.89858719658941E-18,0.005));
#9371=CARTESIAN_POINT('',(0.04,-4.89858719658941E-18,0.015));
#9372=CARTESIAN_POINT('Origin',(0.,0.,0.005));
#9373=CARTESIAN_POINT('Origin',(3.17454396103755E-18,1.73472347597681E-20,
-0.005));
#9374=CARTESIAN_POINT('',(0.026944864,0.017,-0.005));
#9375=CARTESIAN_POINT('Origin',(0.029444864,0.017,-0.005));
#9376=CARTESIAN_POINT('',(0.026944864,-0.017,-0.005));
#9377=CARTESIAN_POINT('Origin',(0.029444864,-0.017,-0.005));
#9378=CARTESIAN_POINT('',(-0.0025,-0.034,-0.005));
#9379=CARTESIAN_POINT('Origin',(-3.46944695195361E-18,-0.034,-0.005));
#9380=CARTESIAN_POINT('',(-0.031944864,-0.017,-0.005));
#9381=CARTESIAN_POINT('Origin',(-0.029444864,-0.017,-0.005));
#9382=CARTESIAN_POINT('',(-0.031944864,0.017,-0.005));
#9383=CARTESIAN_POINT('Origin',(-0.029444864,0.017,-0.005));
#9384=CARTESIAN_POINT('',(-0.0025,0.034,-0.005));
#9385=CARTESIAN_POINT('Origin',(-3.46944695195361E-18,0.034,-0.005));
#9386=CARTESIAN_POINT('',(0.028,-3.42901103761259E-18,-0.005));
#9387=CARTESIAN_POINT('Origin',(0.,0.,-0.005));
#9388=CARTESIAN_POINT('Origin',(3.17454396103755E-18,1.73472347597681E-20,
0.005));
#9389=CARTESIAN_POINT('',(0.026944864,0.017,0.005));
#9390=CARTESIAN_POINT('Origin',(0.029444864,0.017,0.005));
#9391=CARTESIAN_POINT('',(0.026944864,-0.017,0.005));
#9392=CARTESIAN_POINT('Origin',(0.029444864,-0.017,0.005));
#9393=CARTESIAN_POINT('',(-0.00250000000000001,-0.034,0.005));
#9394=CARTESIAN_POINT('Origin',(-6.93889390390723E-18,-0.034,0.005));
#9395=CARTESIAN_POINT('',(-0.031944864,-0.017,0.005));
#9396=CARTESIAN_POINT('Origin',(-0.029444864,-0.017,0.005));
#9397=CARTESIAN_POINT('',(-0.031944864,0.017,0.005));
#9398=CARTESIAN_POINT('Origin',(-0.029444864,0.017,0.005));
#9399=CARTESIAN_POINT('',(-0.00250000000000001,0.034,0.005));
#9400=CARTESIAN_POINT('Origin',(-6.93889390390723E-18,0.034,0.005));
#9401=CARTESIAN_POINT('',(0.028,-3.42901103761259E-18,0.005));
#9402=CARTESIAN_POINT('Origin',(0.,0.,0.005));
#9403=CARTESIAN_POINT('Origin',(0.,0.,0.0065));
#9404=CARTESIAN_POINT('',(0.028,-3.42901103761259E-18,-0.0065));
#9405=CARTESIAN_POINT('Origin',(0.,0.,-0.0065));
#9406=CARTESIAN_POINT('',(0.028,-3.42901103761259E-18,0.0065));
#9407=CARTESIAN_POINT('Origin',(-1.44987137336516E-49,0.034,-0.015));
#9408=CARTESIAN_POINT('',(-0.0025,0.034,-0.015));
#9409=CARTESIAN_POINT('Origin',(-0.029444864,0.017,-0.015));
#9410=CARTESIAN_POINT('',(-0.031944864,0.017,-0.015));
#9411=CARTESIAN_POINT('Origin',(-0.029444864,-0.017,-0.015));
#9412=CARTESIAN_POINT('',(-0.031944864,-0.017,-0.015));
#9413=CARTESIAN_POINT('Origin',(-1.44987137336516E-49,-0.034,-0.015));
#9414=CARTESIAN_POINT('',(-0.0025,-0.034,-0.015));
#9415=CARTESIAN_POINT('Origin',(0.029444864,-0.017,-0.015));
#9416=CARTESIAN_POINT('',(0.026944864,-0.017,-0.015));
#9417=CARTESIAN_POINT('Origin',(0.029444864,0.017,-0.015));
#9418=CARTESIAN_POINT('',(0.026944864,0.017,-0.015));
#9419=CARTESIAN_POINT('Origin',(0.,0.,0.0065));
#9420=CARTESIAN_POINT('',(0.028,-3.42901103761259E-18,0.0065));
#9421=CARTESIAN_POINT('',(0.028,-3.42901103761259E-18,0.0065));
#9422=CARTESIAN_POINT('Origin',(0.,0.,0.0065));
#9423=CARTESIAN_POINT('Origin',(-1.21430643318376E-19,-1.12757025938492E-18,
-0.0065));
#9424=CARTESIAN_POINT('Origin',(-1.21430643318376E-19,-1.12757025938492E-18,
0.0065));
#9425=CARTESIAN_POINT('',(0.,0.,0.));
#9426=CARTESIAN_POINT('Origin',(-0.00639999889435817,-1.33725586897056E-10,
-2.60202312123977E-18));
#9427=CARTESIAN_POINT('',(-0.00750000021337694,-2.62982038223811E-17,-0.0248999997701383));
#9428=CARTESIAN_POINT('',(-0.00750000021337694,-9.33158505355009E-18,0.0248999997701383));
#9429=CARTESIAN_POINT('Origin',(-0.00750000021337694,-1.38314833296201E-10,
-2.61316366403604E-18));
#9430=CARTESIAN_POINT('',(-0.00639999976976533,-1.58005919577827E-12,0.0260000002475909));
#9431=CARTESIAN_POINT('Origin',(-0.00639999889435817,-9.20581548326642E-13,
0.0248999989285722));
#9432=CARTESIAN_POINT('',(-0.00639999976976533,-3.35121902792442E-17,-0.0260000002475909));
#9433=CARTESIAN_POINT('Origin',(-0.00639999977013826,-1.33725590550843E-10,
-2.60202313010945E-18));
#9434=CARTESIAN_POINT('Origin',(-0.00639999889435817,-9.20629689158185E-13,
-0.0248999989285722));
#9435=CARTESIAN_POINT('Origin',(-0.00639999889435817,1.33725588194013E-10,
-2.25687613815873E-19));
#9436=CARTESIAN_POINT('Origin',(-0.00750000021337694,1.38314834487708E-10,
-2.3310041583336E-19));
#9437=CARTESIAN_POINT('Origin',(-0.00639999977013826,1.3372558821988E-10,
4.44089209850063E-18));
#9438=CARTESIAN_POINT('Origin',(-0.0206375,0.,-4.33144407778805E-52));
#9439=CARTESIAN_POINT('',(0.00639999998722997,-6.70342338705283E-12,0.0260000000825303));
#9440=CARTESIAN_POINT('',(0.00639999998722997,-5.37097589710219E-12,-0.0260000000825303));
#9441=CARTESIAN_POINT('Origin',(0.0064,0.,-9.01972807340825E-19));
#9442=CARTESIAN_POINT('Origin',(0.0064,2.91826343292479E-18,0.));
#9443=CARTESIAN_POINT('',(-0.0206375,-3.18408167778312E-18,0.026));
#9444=CARTESIAN_POINT('Origin',(-0.0075,-1.31838984174237E-18,-1.2490009027033E-18));
#9445=CARTESIAN_POINT('',(-0.0075,-2.50440270425634E-18,0.02045));
#9446=CARTESIAN_POINT('Origin',(-0.0075,0.,0.));
#9447=CARTESIAN_POINT('Origin',(0.00639999889435816,-1.33725593635445E-10,
-3.59711256079879E-19));
#9448=CARTESIAN_POINT('',(0.00750000021337694,-1.05191955076574E-17,0.0248999997701383));
#9449=CARTESIAN_POINT('Origin',(0.00639999889435816,-9.20588335445364E-13,
0.0248999989285722));
#9450=CARTESIAN_POINT('',(0.00750000021337694,-2.93287844693988E-17,-0.0248999997701383));
#9451=CARTESIAN_POINT('Origin',(0.00750000021337694,-1.38314840140043E-10,
-3.71488919652902E-19));
#9452=CARTESIAN_POINT('Origin',(0.00639999889435816,-9.20608946339399E-13,
-0.0248999989285722));
#9453=CARTESIAN_POINT('Origin',(-0.0206375,0.,0.));
#9454=CARTESIAN_POINT('',(-0.00413672599961696,1.0458235455062E-18,0.0204500000364447));
#9455=CARTESIAN_POINT('',(-0.0206375,-2.50440270425634E-18,0.02045));
#9456=CARTESIAN_POINT('',(-0.004136726,-0.02045,-2.79956704802153E-18));
#9457=CARTESIAN_POINT('Origin',(-0.004136726,1.15025496390116E-19,8.88178419700125E-18));
#9458=CARTESIAN_POINT('Origin',(-0.004136726,1.15025496390116E-19,8.88178419700125E-18));
#9459=CARTESIAN_POINT('Origin',(0.00639999889435816,1.33725592594967E-10,
2.43522299685913E-19));
#9460=CARTESIAN_POINT('Origin',(0.00750000021337694,1.3831483908365E-10,
2.45725725091783E-19));
#9461=CARTESIAN_POINT('Origin',(0.0075,-1.31838984174237E-18,1.2490009027033E-18));
#9462=CARTESIAN_POINT('',(0.0075,-2.50440270425634E-18,0.02045));
#9463=CARTESIAN_POINT('Origin',(0.0075,0.,0.));
#9464=CARTESIAN_POINT('Origin',(4.25120033285821E-10,2.32696931299848E-18,
-2.53637255105429E-19));
#9465=CARTESIAN_POINT('',(-0.00413672599923392,-0.0130499999271107,-1.89332840771843E-18));
#9466=CARTESIAN_POINT('Origin',(4.25120034352053E-10,-0.01675,-2.30492064367725E-18));
#9467=CARTESIAN_POINT('',(-0.00413672599923392,-9.72427111671565E-12,0.0130499999635554));
#9468=CARTESIAN_POINT('Origin',(-0.00413672599923392,-2.48296911984889E-18,
-8.56610574398074E-20));
#9469=CARTESIAN_POINT('Origin',(-0.00413672599923392,-2.48296911984889E-18,
-8.56610574398074E-20));
#9470=CARTESIAN_POINT('Origin',(-0.0206375,0.,0.));
#9471=CARTESIAN_POINT('',(0.004136726,-0.02045,-1.97855791081413E-18));
#9472=CARTESIAN_POINT('',(0.004136726,-2.50440270425634E-18,0.02045));
#9473=CARTESIAN_POINT('Origin',(0.004136726,-1.49874617044541E-18,-8.88178419700125E-18));
#9474=CARTESIAN_POINT('Origin',(0.004136726,-1.49874617044541E-18,-8.88178419700125E-18));
#9475=CARTESIAN_POINT('',(-0.0206375,-2.50440270425634E-18,0.02045));
#9476=CARTESIAN_POINT('Origin',(-0.0206375,0.,0.));
#9477=CARTESIAN_POINT('',(-0.0075,-1.5981640728873E-18,0.01305));
#9478=CARTESIAN_POINT('',(-0.0206375,-1.5981640728873E-18,0.01305));
#9479=CARTESIAN_POINT('Origin',(-0.0075,0.,0.));
#9480=CARTESIAN_POINT('Origin',(-4.25120036303284E-10,3.75386134271222E-18,
6.07632462000188E-19));
#9481=CARTESIAN_POINT('',(0.00413672599923392,-2.67659699192252E-12,0.0130499999635553));
#9482=CARTESIAN_POINT('',(0.00413672599923392,-0.01305,-1.07231927942994E-18));
#9483=CARTESIAN_POINT('Origin',(0.00413672599923392,-3.3221160294436E-19,
2.22044604925031E-18));
#9484=CARTESIAN_POINT('Origin',(-4.25120034317525E-10,-0.01675,-1.44365092657163E-18));
#9485=CARTESIAN_POINT('Origin',(0.00413672599923392,-3.3221160294436E-19,
2.22044604925031E-18));
#9486=CARTESIAN_POINT('Origin',(-0.0075,-1.3010426069826E-19,-1.1666015375944E-18));
#9487=CARTESIAN_POINT('',(-0.00750000021337695,-7.32444758467801E-18,-0.00860000022986174));
#9488=CARTESIAN_POINT('',(-0.00750000021337695,-9.55563692214474E-13,0.00860000022983698));
#9489=CARTESIAN_POINT('Origin',(-0.00750000021337695,1.20438122996688E-10,
1.91155415755433E-19));
#9490=CARTESIAN_POINT('Origin',(-0.00750000021337695,-1.20438124044286E-10,
-1.263242268E-19));
#9491=CARTESIAN_POINT('Origin',(-0.0206375,0.,0.));
#9492=CARTESIAN_POINT('',(0.0075,-1.5981640728873E-18,0.01305));
#9493=CARTESIAN_POINT('Origin',(0.0075,0.,0.));
#9494=CARTESIAN_POINT('',(-0.0206375,-1.5981640728873E-18,0.01305));
#9495=CARTESIAN_POINT('Origin',(-0.00639999889435815,-1.33725589876008E-10,
-1.99489279445979E-19));
#9496=CARTESIAN_POINT('',(-0.00639999933187528,-1.78004529143068E-13,0.00749999975240887));
#9497=CARTESIAN_POINT('Origin',(-0.00639999889435815,-4.29138899262724E-13,
0.00860000107142784));
#9498=CARTESIAN_POINT('',(-0.00639999933187528,7.82593383085413E-14,-0.00749999975240887));
#9499=CARTESIAN_POINT('Origin',(-0.00639999977013826,-1.33725577217623E-10,
-2.22044604925031E-18));
#9500=CARTESIAN_POINT('Origin',(-0.00639999889435815,-4.29112928832131E-13,
-0.00860000107142784));
#9501=CARTESIAN_POINT('Origin',(-0.00639999889435816,1.33725589406987E-10,
2.62934110861178E-19));
#9502=CARTESIAN_POINT('Origin',(-0.00639999889435816,1.33725589406987E-10,
2.62934110861178E-19));
#9503=CARTESIAN_POINT('Origin',(0.0075,-1.3010426069826E-19,1.1666015375944E-18));
#9504=CARTESIAN_POINT('',(0.00750000021337695,-1.12844211802569E-18,0.00860000022986174));
#9505=CARTESIAN_POINT('',(0.00750000021337695,-9.55567354576375E-13,-0.00860000022983698));
#9506=CARTESIAN_POINT('Origin',(0.00750000021337695,1.20438122943562E-10,
-1.36910420000699E-19));
#9507=CARTESIAN_POINT('Origin',(0.00750000021337695,-1.20438123513651E-10,
2.9038238015475E-19));
#9508=CARTESIAN_POINT('Origin',(-0.0206375,0.,-2.49552314011156E-51));
#9509=CARTESIAN_POINT('',(0.00639999944717908,-3.41326938021997E-12,0.00749999987620436));
#9510=CARTESIAN_POINT('',(-0.0206375,-9.18485099360515E-19,0.0075));
#9511=CARTESIAN_POINT('',(0.00639999944670613,1.23481356905966E-13,-0.0074999998349392));
#9512=CARTESIAN_POINT('Origin',(0.0064,-1.93061231994698E-18,-5.55111512312578E-18));
#9513=CARTESIAN_POINT('Origin',(0.00639999889435815,1.33725588774518E-10,
-1.62015184442301E-19));
#9514=CARTESIAN_POINT('Origin',(0.00639999889435815,-1.33725589355705E-10,
3.07932432666985E-19));
#9515=CARTESIAN_POINT('Origin',(0.00639999889435815,-4.29128599184298E-13,
0.00860000107142785));
#9516=CARTESIAN_POINT('Origin',(0.00639999889435815,-4.2911240869608E-13,
-0.00860000107142785));
#9517=CARTESIAN_POINT('Origin',(0.00639999889435815,1.33725588774518E-10,
-1.62015184442301E-19));
#9518=CARTESIAN_POINT('',(0.,0.,0.));
#9519=CARTESIAN_POINT('Origin',(-0.00639999889435817,-1.33725586897056E-10,
-2.60202312123977E-18));
#9520=CARTESIAN_POINT('',(-0.00750000021337694,-2.62982038223811E-17,-0.0248999997701383));
#9521=CARTESIAN_POINT('',(-0.00750000021337694,-9.33158505355009E-18,0.0248999997701383));
#9522=CARTESIAN_POINT('Origin',(-0.00750000021337694,-1.38314833296201E-10,
-2.61316366403604E-18));
#9523=CARTESIAN_POINT('',(-0.00639999976976533,-1.58005919577827E-12,0.0260000002475909));
#9524=CARTESIAN_POINT('Origin',(-0.00639999889435817,-9.20581548326642E-13,
0.0248999989285722));
#9525=CARTESIAN_POINT('',(-0.00639999976976533,-3.35121902792442E-17,-0.0260000002475909));
#9526=CARTESIAN_POINT('Origin',(-0.00639999977013826,-1.33725590550843E-10,
-2.60202313010945E-18));
#9527=CARTESIAN_POINT('Origin',(-0.00639999889435817,-9.20629689158185E-13,
-0.0248999989285722));
#9528=CARTESIAN_POINT('Origin',(-0.00639999889435817,1.33725588194013E-10,
-2.25687613815873E-19));
#9529=CARTESIAN_POINT('Origin',(-0.00750000021337694,1.38314834487708E-10,
-2.3310041583336E-19));
#9530=CARTESIAN_POINT('Origin',(-0.00639999977013826,1.3372558821988E-10,
4.44089209850063E-18));
#9531=CARTESIAN_POINT('Origin',(-0.0206375,0.,-4.33144407778805E-52));
#9532=CARTESIAN_POINT('',(0.00639999998722997,-6.70342338705283E-12,0.0260000000825303));
#9533=CARTESIAN_POINT('',(0.00639999998722997,-5.37097589710219E-12,-0.0260000000825303));
#9534=CARTESIAN_POINT('Origin',(0.0064,0.,-9.01972807340825E-19));
#9535=CARTESIAN_POINT('Origin',(0.0064,2.91826343292479E-18,0.));
#9536=CARTESIAN_POINT('',(-0.0206375,-3.18408167778312E-18,0.026));
#9537=CARTESIAN_POINT('Origin',(-0.0075,-1.31838984174237E-18,-1.2490009027033E-18));
#9538=CARTESIAN_POINT('',(-0.0075,-2.50440270425634E-18,0.02045));
#9539=CARTESIAN_POINT('Origin',(-0.0075,0.,0.));
#9540=CARTESIAN_POINT('Origin',(0.00639999889435816,-1.33725593635445E-10,
-3.59711256079879E-19));
#9541=CARTESIAN_POINT('',(0.00750000021337694,-1.05191955076574E-17,0.0248999997701383));
#9542=CARTESIAN_POINT('Origin',(0.00639999889435816,-9.20588335445364E-13,
0.0248999989285722));
#9543=CARTESIAN_POINT('',(0.00750000021337694,-2.93287844693988E-17,-0.0248999997701383));
#9544=CARTESIAN_POINT('Origin',(0.00750000021337694,-1.38314840140043E-10,
-3.71488919652902E-19));
#9545=CARTESIAN_POINT('Origin',(0.00639999889435816,-9.20608946339399E-13,
-0.0248999989285722));
#9546=CARTESIAN_POINT('Origin',(-0.0206375,0.,0.));
#9547=CARTESIAN_POINT('',(-0.00413672599961696,1.0458235455062E-18,0.0204500000364447));
#9548=CARTESIAN_POINT('',(-0.0206375,-2.50440270425634E-18,0.02045));
#9549=CARTESIAN_POINT('',(-0.004136726,-0.02045,-2.79956704802153E-18));
#9550=CARTESIAN_POINT('Origin',(-0.004136726,1.15025496390116E-19,8.88178419700125E-18));
#9551=CARTESIAN_POINT('Origin',(-0.004136726,1.15025496390116E-19,8.88178419700125E-18));
#9552=CARTESIAN_POINT('Origin',(0.00639999889435816,1.33725592594967E-10,
2.43522299685913E-19));
#9553=CARTESIAN_POINT('Origin',(0.00750000021337694,1.3831483908365E-10,
2.45725725091783E-19));
#9554=CARTESIAN_POINT('Origin',(0.0075,-1.31838984174237E-18,1.2490009027033E-18));
#9555=CARTESIAN_POINT('',(0.0075,-2.50440270425634E-18,0.02045));
#9556=CARTESIAN_POINT('Origin',(0.0075,0.,0.));
#9557=CARTESIAN_POINT('Origin',(4.25120033285821E-10,2.32696931299848E-18,
-2.53637255105429E-19));
#9558=CARTESIAN_POINT('',(-0.00413672599923392,-0.0130499999271107,-1.89332840771843E-18));
#9559=CARTESIAN_POINT('Origin',(4.25120034352053E-10,-0.01675,-2.30492064367725E-18));
#9560=CARTESIAN_POINT('',(-0.00413672599923392,-9.72427111671565E-12,0.0130499999635554));
#9561=CARTESIAN_POINT('Origin',(-0.00413672599923392,-2.48296911984889E-18,
-8.56610574398074E-20));
#9562=CARTESIAN_POINT('Origin',(-0.00413672599923392,-2.48296911984889E-18,
-8.56610574398074E-20));
#9563=CARTESIAN_POINT('Origin',(-0.0206375,0.,0.));
#9564=CARTESIAN_POINT('',(0.004136726,-0.02045,-1.97855791081413E-18));
#9565=CARTESIAN_POINT('',(0.004136726,-2.50440270425634E-18,0.02045));
#9566=CARTESIAN_POINT('Origin',(0.004136726,-1.49874617044541E-18,-8.88178419700125E-18));
#9567=CARTESIAN_POINT('Origin',(0.004136726,-1.49874617044541E-18,-8.88178419700125E-18));
#9568=CARTESIAN_POINT('',(-0.0206375,-2.50440270425634E-18,0.02045));
#9569=CARTESIAN_POINT('Origin',(-0.0206375,0.,0.));
#9570=CARTESIAN_POINT('',(-0.0075,-1.5981640728873E-18,0.01305));
#9571=CARTESIAN_POINT('',(-0.0206375,-1.5981640728873E-18,0.01305));
#9572=CARTESIAN_POINT('Origin',(-0.0075,0.,0.));
#9573=CARTESIAN_POINT('Origin',(-4.25120036303284E-10,3.75386134271222E-18,
6.07632462000188E-19));
#9574=CARTESIAN_POINT('',(0.00413672599923392,-2.67659699192252E-12,0.0130499999635553));
#9575=CARTESIAN_POINT('',(0.00413672599923392,-0.01305,-1.07231927942994E-18));
#9576=CARTESIAN_POINT('Origin',(0.00413672599923392,-3.3221160294436E-19,
2.22044604925031E-18));
#9577=CARTESIAN_POINT('Origin',(-4.25120034317525E-10,-0.01675,-1.44365092657163E-18));
#9578=CARTESIAN_POINT('Origin',(0.00413672599923392,-3.3221160294436E-19,
2.22044604925031E-18));
#9579=CARTESIAN_POINT('Origin',(-0.0075,-1.3010426069826E-19,-1.1666015375944E-18));
#9580=CARTESIAN_POINT('',(-0.00750000021337695,-7.32444758467801E-18,-0.00860000022986174));
#9581=CARTESIAN_POINT('',(-0.00750000021337695,-9.55563692214474E-13,0.00860000022983698));
#9582=CARTESIAN_POINT('Origin',(-0.00750000021337695,1.20438122996688E-10,
1.91155415755433E-19));
#9583=CARTESIAN_POINT('Origin',(-0.00750000021337695,-1.20438124044286E-10,
-1.263242268E-19));
#9584=CARTESIAN_POINT('Origin',(-0.0206375,0.,0.));
#9585=CARTESIAN_POINT('',(0.0075,-1.5981640728873E-18,0.01305));
#9586=CARTESIAN_POINT('Origin',(0.0075,0.,0.));
#9587=CARTESIAN_POINT('',(-0.0206375,-1.5981640728873E-18,0.01305));
#9588=CARTESIAN_POINT('Origin',(-0.00639999889435815,-1.33725589876008E-10,
-1.99489279445979E-19));
#9589=CARTESIAN_POINT('',(-0.00639999933187528,-1.78004529143068E-13,0.00749999975240887));
#9590=CARTESIAN_POINT('Origin',(-0.00639999889435815,-4.29138899262724E-13,
0.00860000107142784));
#9591=CARTESIAN_POINT('',(-0.00639999933187528,7.82593383085413E-14,-0.00749999975240887));
#9592=CARTESIAN_POINT('Origin',(-0.00639999977013826,-1.33725577217623E-10,
-2.22044604925031E-18));
#9593=CARTESIAN_POINT('Origin',(-0.00639999889435815,-4.29112928832131E-13,
-0.00860000107142784));
#9594=CARTESIAN_POINT('Origin',(-0.00639999889435816,1.33725589406987E-10,
2.62934110861178E-19));
#9595=CARTESIAN_POINT('Origin',(-0.00639999889435816,1.33725589406987E-10,
2.62934110861178E-19));
#9596=CARTESIAN_POINT('Origin',(0.0075,-1.3010426069826E-19,1.1666015375944E-18));
#9597=CARTESIAN_POINT('',(0.00750000021337695,-1.12844211802569E-18,0.00860000022986174));
#9598=CARTESIAN_POINT('',(0.00750000021337695,-9.55567354576375E-13,-0.00860000022983698));
#9599=CARTESIAN_POINT('Origin',(0.00750000021337695,1.20438122943562E-10,
-1.36910420000699E-19));
#9600=CARTESIAN_POINT('Origin',(0.00750000021337695,-1.20438123513651E-10,
2.9038238015475E-19));
#9601=CARTESIAN_POINT('Origin',(-0.0206375,0.,-2.49552314011156E-51));
#9602=CARTESIAN_POINT('',(0.00639999944717908,-3.41326938021997E-12,0.00749999987620436));
#9603=CARTESIAN_POINT('',(-0.0206375,-9.18485099360515E-19,0.0075));
#9604=CARTESIAN_POINT('',(0.00639999944670613,1.23481356905966E-13,-0.0074999998349392));
#9605=CARTESIAN_POINT('Origin',(0.0064,-1.93061231994698E-18,-5.55111512312578E-18));
#9606=CARTESIAN_POINT('Origin',(0.00639999889435815,1.33725588774518E-10,
-1.62015184442301E-19));
#9607=CARTESIAN_POINT('Origin',(0.00639999889435815,-1.33725589355705E-10,
3.07932432666985E-19));
#9608=CARTESIAN_POINT('Origin',(0.00639999889435815,-4.29128599184298E-13,
0.00860000107142785));
#9609=CARTESIAN_POINT('Origin',(0.00639999889435815,-4.2911240869608E-13,
-0.00860000107142785));
#9610=CARTESIAN_POINT('Origin',(0.00639999889435815,1.33725588774518E-10,
-1.62015184442301E-19));
#9611=CARTESIAN_POINT('',(0.,0.,0.));
#9612=CARTESIAN_POINT('Origin',(-5.74005956283549E-52,0.,0.015));
#9613=CARTESIAN_POINT('',(-0.042,-1.9853686361416E-11,0.007381198));
#9614=CARTESIAN_POINT('Origin',(-2.66453525910038E-17,5.09119415777057E-18,
0.007381198));
#9615=CARTESIAN_POINT('',(-0.042,-1.54820701770975E-11,-0.007381198));
#9616=CARTESIAN_POINT('',(-0.042,-5.14351655641888E-18,0.015));
#9617=CARTESIAN_POINT('',(0.0419999999999985,-5.1435165564187E-18,-0.00738119800000199));
#9618=CARTESIAN_POINT('Origin',(-8.88178419700125E-18,-5.73557577313579E-18,
-0.007381198));
#9619=CARTESIAN_POINT('Origin',(-8.88178419700125E-18,-5.73557577313579E-18,
-0.007381198));
#9620=CARTESIAN_POINT('Origin',(-2.64244881468667E-16,0.,-0.560482737499999));
#9621=CARTESIAN_POINT('',(0.0499999999999997,-6.12323399573673E-18,-0.0120000000000027));
#9622=CARTESIAN_POINT('Origin',(8.88178419700125E-18,1.23918456012259E-18,
-0.012000000000002));
#9623=CARTESIAN_POINT('',(1.,-1.22464679914735E-16,-0.5604827375));
#9624=CARTESIAN_POINT('Origin',(2.63459037944631E-16,0.,0.560482737500119));
#9625=CARTESIAN_POINT('',(0.05,-2.05102985990085E-11,0.0120000000000921));
#9626=CARTESIAN_POINT('',(-0.0499999999999868,-6.12323399573515E-18,0.0120000000001151));
#9627=CARTESIAN_POINT('Origin',(1.77635683940025E-17,-6.31136467490802E-18,
0.0120000000000921));
#9628=CARTESIAN_POINT('',(-1.,-1.22464679914735E-16,0.560482737500119));
#9629=CARTESIAN_POINT('Origin',(1.77635683940025E-17,-6.31136467490802E-18,
0.0120000000000921));
#9630=CARTESIAN_POINT('Origin',(0.,0.,0.015));
#9631=CARTESIAN_POINT('',(0.05,-6.12323399573677E-18,-0.015));
#9632=CARTESIAN_POINT('Origin',(0.,0.,-0.015));
#9633=CARTESIAN_POINT('',(0.05,-6.12323399573677E-18,0.015));
#9634=CARTESIAN_POINT('Origin',(0.,0.,0.015));
#9635=CARTESIAN_POINT('',(0.05,-6.12323399573677E-18,0.015));
#9636=CARTESIAN_POINT('',(0.05,-6.12323399573677E-18,0.015));
#9637=CARTESIAN_POINT('Origin',(0.,0.,0.015));
#9638=CARTESIAN_POINT('Origin',(5.79397640976254E-18,1.73472347597681E-19,
-0.015));
#9639=CARTESIAN_POINT('',(0.04,-4.89858719658941E-18,-0.015));
#9640=CARTESIAN_POINT('Origin',(-6.50521303491303E-19,0.,-0.015));
#9641=CARTESIAN_POINT('Origin',(5.79397640976254E-18,1.73472347597681E-19,
0.015));
#9642=CARTESIAN_POINT('',(0.04,-4.89858719658941E-18,0.015));
#9643=CARTESIAN_POINT('Origin',(0.,0.,0.015));
#9644=CARTESIAN_POINT('Origin',(1.85684700327654E-52,0.,0.015));
#9645=CARTESIAN_POINT('',(0.04,-4.89858719658941E-18,-0.005));
#9646=CARTESIAN_POINT('Origin',(-4.33680868994202E-19,0.,-0.005));
#9647=CARTESIAN_POINT('',(0.04,-4.89858719658941E-18,0.015));
#9648=CARTESIAN_POINT('Origin',(0.,0.,0.015));
#9649=CARTESIAN_POINT('',(0.04,-4.89858719658941E-18,0.005));
#9650=CARTESIAN_POINT('',(0.04,-4.89858719658941E-18,0.015));
#9651=CARTESIAN_POINT('Origin',(0.,0.,0.005));
#9652=CARTESIAN_POINT('Origin',(3.17454396103755E-18,1.73472347597681E-20,
-0.005));
#9653=CARTESIAN_POINT('',(0.026944864,0.017,-0.005));
#9654=CARTESIAN_POINT('Origin',(0.029444864,0.017,-0.005));
#9655=CARTESIAN_POINT('',(0.026944864,-0.017,-0.005));
#9656=CARTESIAN_POINT('Origin',(0.029444864,-0.017,-0.005));
#9657=CARTESIAN_POINT('',(-0.0025,-0.034,-0.005));
#9658=CARTESIAN_POINT('Origin',(-3.46944695195361E-18,-0.034,-0.005));
#9659=CARTESIAN_POINT('',(-0.031944864,-0.017,-0.005));
#9660=CARTESIAN_POINT('Origin',(-0.029444864,-0.017,-0.005));
#9661=CARTESIAN_POINT('',(-0.031944864,0.017,-0.005));
#9662=CARTESIAN_POINT('Origin',(-0.029444864,0.017,-0.005));
#9663=CARTESIAN_POINT('',(-0.0025,0.034,-0.005));
#9664=CARTESIAN_POINT('Origin',(-3.46944695195361E-18,0.034,-0.005));
#9665=CARTESIAN_POINT('',(0.028,-3.42901103761259E-18,-0.005));
#9666=CARTESIAN_POINT('Origin',(0.,0.,-0.005));
#9667=CARTESIAN_POINT('Origin',(3.17454396103755E-18,1.73472347597681E-20,
0.005));
#9668=CARTESIAN_POINT('',(0.026944864,0.017,0.005));
#9669=CARTESIAN_POINT('Origin',(0.029444864,0.017,0.005));
#9670=CARTESIAN_POINT('',(0.026944864,-0.017,0.005));
#9671=CARTESIAN_POINT('Origin',(0.029444864,-0.017,0.005));
#9672=CARTESIAN_POINT('',(-0.00250000000000001,-0.034,0.005));
#9673=CARTESIAN_POINT('Origin',(-6.93889390390723E-18,-0.034,0.005));
#9674=CARTESIAN_POINT('',(-0.031944864,-0.017,0.005));
#9675=CARTESIAN_POINT('Origin',(-0.029444864,-0.017,0.005));
#9676=CARTESIAN_POINT('',(-0.031944864,0.017,0.005));
#9677=CARTESIAN_POINT('Origin',(-0.029444864,0.017,0.005));
#9678=CARTESIAN_POINT('',(-0.00250000000000001,0.034,0.005));
#9679=CARTESIAN_POINT('Origin',(-6.93889390390723E-18,0.034,0.005));
#9680=CARTESIAN_POINT('',(0.028,-3.42901103761259E-18,0.005));
#9681=CARTESIAN_POINT('Origin',(0.,0.,0.005));
#9682=CARTESIAN_POINT('Origin',(0.,0.,0.0065));
#9683=CARTESIAN_POINT('',(0.028,-3.42901103761259E-18,-0.0065));
#9684=CARTESIAN_POINT('Origin',(0.,0.,-0.0065));
#9685=CARTESIAN_POINT('',(0.028,-3.42901103761259E-18,0.0065));
#9686=CARTESIAN_POINT('Origin',(-1.44987137336516E-49,0.034,-0.015));
#9687=CARTESIAN_POINT('',(-0.0025,0.034,-0.015));
#9688=CARTESIAN_POINT('Origin',(-0.029444864,0.017,-0.015));
#9689=CARTESIAN_POINT('',(-0.031944864,0.017,-0.015));
#9690=CARTESIAN_POINT('Origin',(-0.029444864,-0.017,-0.015));
#9691=CARTESIAN_POINT('',(-0.031944864,-0.017,-0.015));
#9692=CARTESIAN_POINT('Origin',(-1.44987137336516E-49,-0.034,-0.015));
#9693=CARTESIAN_POINT('',(-0.0025,-0.034,-0.015));
#9694=CARTESIAN_POINT('Origin',(0.029444864,-0.017,-0.015));
#9695=CARTESIAN_POINT('',(0.026944864,-0.017,-0.015));
#9696=CARTESIAN_POINT('Origin',(0.029444864,0.017,-0.015));
#9697=CARTESIAN_POINT('',(0.026944864,0.017,-0.015));
#9698=CARTESIAN_POINT('Origin',(0.,0.,0.0065));
#9699=CARTESIAN_POINT('',(0.028,-3.42901103761259E-18,0.0065));
#9700=CARTESIAN_POINT('',(0.028,-3.42901103761259E-18,0.0065));
#9701=CARTESIAN_POINT('Origin',(0.,0.,0.0065));
#9702=CARTESIAN_POINT('Origin',(-1.21430643318376E-19,-1.12757025938492E-18,
-0.0065));
#9703=CARTESIAN_POINT('',(0.025,-3.06161699786838E-18,-0.0065));
#9704=CARTESIAN_POINT('Origin',(0.,0.,-0.0065));
#9705=CARTESIAN_POINT('Origin',(-1.21430643318376E-19,-1.12757025938492E-18,
0.0065));
#9706=CARTESIAN_POINT('',(0.025,-3.06161699786838E-18,0.0065));
#9707=CARTESIAN_POINT('Origin',(0.,0.,0.0065));
#9708=CARTESIAN_POINT('Origin',(0.,0.,0.0065));
#9709=CARTESIAN_POINT('',(0.025,-3.06161699786838E-18,0.0065));
#9710=CARTESIAN_POINT('',(0.,0.,0.));
#9711=CARTESIAN_POINT('Origin',(0.,0.,-7.87263173541793E-35));
#9712=CARTESIAN_POINT('',(-0.0233679536357646,-0.034898979153486,-0.00737500014596191));
#9713=CARTESIAN_POINT('',(0.0233679535551443,0.0348989792127245,-0.00737499998943404));
#9714=CARTESIAN_POINT('Origin',(4.44089209850063E-17,-3.10862446895044E-17,
-0.007375));
#9715=CARTESIAN_POINT('',(-0.0233679536079189,-0.0348989791421631,0.00737500011314446));
#9716=CARTESIAN_POINT('',(-0.0233679535483332,-0.0348989791679204,-0.00737499975));
#9717=CARTESIAN_POINT('',(0.0233679535131933,0.0348989792427655,0.00737499998724119));
#9718=CARTESIAN_POINT('Origin',(1.77635683940025E-17,8.88178419700125E-18,
0.007375));
#9719=CARTESIAN_POINT('',(0.023367953562649,0.0348989791583347,0.00737499975));
#9720=CARTESIAN_POINT('Origin',(-0.526632046,0.40317263,-3.19189119579732E-18));
#9721=CARTESIAN_POINT('',(-1.0766320462855,0.771446280610377,0.00737500043869704));
#9722=CARTESIAN_POINT('',(-1.07663204595213,0.771446280476663,0.00737500070705611));
#9723=CARTESIAN_POINT('',(-1.07663204628435,0.771446280609598,-0.00737500043868999));
#9724=CARTESIAN_POINT('',(-1.076632046,0.771446281,-0.00737499999631251));
#9725=CARTESIAN_POINT('',(0.0233679534964875,0.034898979368365,-0.00737499995506969));
#9726=CARTESIAN_POINT('Origin',(0.,0.,0.560476539500209));
#9727=CARTESIAN_POINT('',(-0.0278189923670676,-0.0415464037720794,0.011993802156313));
#9728=CARTESIAN_POINT('',(-0.0233679536799733,-0.034898979364519,0.00737500013681456));
#9729=CARTESIAN_POINT('',(0.0278189923276001,0.0415464037677099,0.0119938019829276));
#9730=CARTESIAN_POINT('Origin',(1.33226762955019E-17,8.88178419700125E-18,
0.0119938020001596));
#9731=CARTESIAN_POINT('',(0.0278189922159758,0.0415464035799445,0.0119938018751596));
#9732=CARTESIAN_POINT('Origin',(0.,0.,-0.560476539500202));
#9733=CARTESIAN_POINT('',(-0.0278189923461909,-0.0415464037862849,-0.0119938021566348));
#9734=CARTESIAN_POINT('',(0.0278189923407346,0.0415464037588361,-0.0119938019828069));
#9735=CARTESIAN_POINT('Origin',(2.66453525910038E-17,1.32781373427172E-17,
-0.0119938020001543));
#9736=CARTESIAN_POINT('',(-0.0278189922085164,-0.041546403584943,-0.0119938018751542));
#9737=CARTESIAN_POINT('',(0.023367953697375,0.0348989793285763,-0.00737500012515425));
#9738=CARTESIAN_POINT('Origin',(-0.524406527000001,0.406496342,0.00968440124999999));
#9739=CARTESIAN_POINT('',(-1.0721810077487,0.778093704786141,0.0119938023047236));
#9740=CARTESIAN_POINT('',(-1.07218100730026,0.778093704531458,0.0119938024396044));
#9741=CARTESIAN_POINT('',(-1.07663204644624,0.77144628044497,0.00737500053312992));
#9742=CARTESIAN_POINT('Origin',(-1.1,0.736547301,-1.65083181236565E-33));
#9743=CARTESIAN_POINT('',(-1.12336795372113,0.701648321968335,-0.00737500014124816));
#9744=CARTESIAN_POINT('',(-1.12336795361188,0.701648321848912,0.00737500010599789));
#9745=CARTESIAN_POINT('',(-1.12336795354833,0.70164832183208,0.00737499975));
#9746=CARTESIAN_POINT('Origin',(-1.1,0.736547301,-0.00737499999999999));
#9747=CARTESIAN_POINT('Origin',(-1.1,0.736547301,0.007375));
#9748=CARTESIAN_POINT('Origin',(-0.524406527000001,0.406496342,-0.00968440125000005));
#9749=CARTESIAN_POINT('',(-1.07218100774996,0.778093704787018,-0.0119938023047757));
#9750=CARTESIAN_POINT('',(0.0278189920263111,0.0415464039823829,-0.0119938019516094));
#9751=CARTESIAN_POINT('',(-1.07218100773738,0.778093704356822,-0.011993802335713));
#9752=CARTESIAN_POINT('Origin',(0.,0.,-2.35699650765267E-35));
#9753=CARTESIAN_POINT('',(-0.0278189923194442,-0.0415464037713338,-0.01199380175));
#9754=CARTESIAN_POINT('',(0.0278189923364869,0.0415464037599223,0.01199380175));
#9755=CARTESIAN_POINT('Origin',(-0.573367954,0.333374671499999,-3.19189119579732E-18));
#9756=CARTESIAN_POINT('',(-0.0233679541909832,-0.0348989786903893,0.00737500026154926));
#9757=CARTESIAN_POINT('',(-1.1233679536435,0.701648321915596,-0.00737500022207161));
#9758=CARTESIAN_POINT('Origin',(-0.575593473000001,0.33005095925,-0.00968440124999998));
#9759=CARTESIAN_POINT('',(-1.12781899223605,0.69500089782109,-0.011993801966612));
#9760=CARTESIAN_POINT('',(-1.12781899190905,0.695000897939099,-0.0119938018658674));
#9761=CARTESIAN_POINT('',(-1.12336795377236,0.701648322288803,-0.00737500008442041));
#9762=CARTESIAN_POINT('Origin',(-0.522181008,0.4098200545,-6.67868538251071E-19));
#9763=CARTESIAN_POINT('',(-1.072181008,0.778093705,0.0119938018623003));
#9764=CARTESIAN_POINT('Origin',(-1.1,0.736547301,0.560476539499858));
#9765=CARTESIAN_POINT('',(-1.12781899207711,0.695000897561786,0.0119938019516492));
#9766=CARTESIAN_POINT('Origin',(-1.1,0.736547301,0.0119938019998959));
#9767=CARTESIAN_POINT('',(-1.1278189920545,0.695000897624348,0.0119938017249309));
#9768=CARTESIAN_POINT('Origin',(-1.1,0.736547301,-0.560476539499883));
#9769=CARTESIAN_POINT('Origin',(-1.09999999999998,0.736547301000009,-0.011993801999925));
#9770=CARTESIAN_POINT('Origin',(-0.575593473000001,0.33005095925,0.00968440125000007));
#9771=CARTESIAN_POINT('',(-0.0278189926997751,-0.0415464035314387,0.0119938023524818));
#9772=CARTESIAN_POINT('Origin',(-0.577818992,0.326727247,-6.67868538251071E-19));
#9773=CARTESIAN_POINT('',(-1.127818992,0.695000898,-0.0119938018016607));
#9774=CARTESIAN_POINT('Origin',(-1.1,0.736547301,-1.37226748941978E-34));
#9775=CARTESIAN_POINT('',(0.,0.,0.));
#9776=CARTESIAN_POINT('Origin',(0.51,-0.312833309,-0.025));
#9777=CARTESIAN_POINT('',(0.51,-0.312833309,-0.03));
#9778=CARTESIAN_POINT('Origin',(0.51,-0.312833309,-0.025));
#9779=CARTESIAN_POINT('',(0.5,-0.312833309,-0.03));
#9780=CARTESIAN_POINT('',(0.51,-0.312833309,-0.03));
#9781=CARTESIAN_POINT('Origin',(0.5,-0.312833309,-0.025));
#9782=CARTESIAN_POINT('Origin',(0.5,-0.353273650499999,5.93275428784068E-18));
#9783=CARTESIAN_POINT('',(0.500000000000024,-0.250000000000504,0.0499999999998374));
#9784=CARTESIAN_POINT('',(0.500000000000024,-0.456547300999497,0.0499999999998374));
#9785=CARTESIAN_POINT('',(0.5,-0.250000000038728,0.05));
#9786=CARTESIAN_POINT('',(0.500000000000024,-0.250000000000504,-0.0499999999998374));
#9787=CARTESIAN_POINT('',(0.5,-0.25,-0.0499999999875));
#9788=CARTESIAN_POINT('',(0.500000000000037,-0.456547300999497,-0.0499999999996342));
#9789=CARTESIAN_POINT('',(0.5,-0.456547300974182,-0.05));
#9790=CARTESIAN_POINT('',(0.5,-0.456547301,0.0499999999875));
#9791=CARTESIAN_POINT('',(0.5,-0.270944436,0.02));
#9792=CARTESIAN_POINT('Origin',(0.5,-0.270944436,0.025));
#9793=CARTESIAN_POINT('',(0.5,-0.386547301,-0.025));
#9794=CARTESIAN_POINT('Origin',(0.5,-0.386547301,0.));
#9795=CARTESIAN_POINT('',(0.5,-0.270944436,-0.03));
#9796=CARTESIAN_POINT('Origin',(0.5,-0.270944436,-0.025));
#9797=CARTESIAN_POINT('',(0.5,-0.312833309,0.02));
#9798=CARTESIAN_POINT('Origin',(0.5,-0.312833309,0.025));
#9799=CARTESIAN_POINT('Origin',(0.51,-0.353273650499999,5.93275428784068E-18));
#9800=CARTESIAN_POINT('',(0.509999999999963,-0.250000000000504,-0.0499999999996342));
#9801=CARTESIAN_POINT('',(0.509999999999963,-0.250000000000504,0.0499999999996342));
#9802=CARTESIAN_POINT('',(0.51,-0.25,-0.04999999998125));
#9803=CARTESIAN_POINT('',(0.509999999999976,-0.456547300999497,0.0499999999998374));
#9804=CARTESIAN_POINT('',(0.51,-0.250000000025819,0.05));
#9805=CARTESIAN_POINT('',(0.509999999999963,-0.456547300999497,-0.0499999999996342));
#9806=CARTESIAN_POINT('',(0.51,-0.456547301,0.0499999999875));
#9807=CARTESIAN_POINT('',(0.51,-0.456547300974182,-0.05));
#9808=CARTESIAN_POINT('',(0.51,-0.270944436,-0.03));
#9809=CARTESIAN_POINT('Origin',(0.51,-0.270944436,-0.025));
#9810=CARTESIAN_POINT('',(0.51,-0.386547301,-0.025));
#9811=CARTESIAN_POINT('Origin',(0.51,-0.386547301,0.));
#9812=CARTESIAN_POINT('',(0.51,-0.270944436,0.02));
#9813=CARTESIAN_POINT('Origin',(0.51,-0.270944436,0.025));
#9814=CARTESIAN_POINT('',(0.51,-0.312833309,0.02));
#9815=CARTESIAN_POINT('Origin',(0.51,-0.312833309,0.025));
#9816=CARTESIAN_POINT('Origin',(0.51,-0.312833309,0.025));
#9817=CARTESIAN_POINT('',(0.51,-0.312833309,0.02));
#9818=CARTESIAN_POINT('Origin',(0.51,-0.270944436,-0.025));
#9819=CARTESIAN_POINT('',(0.51,-0.270944436,-0.03));
#9820=CARTESIAN_POINT('Origin',(0.51,-0.386547301,0.));
#9821=CARTESIAN_POINT('',(0.51,-0.386547301,-0.025));
#9822=CARTESIAN_POINT('Origin',(0.51,-0.270944436,0.025));
#9823=CARTESIAN_POINT('',(0.51,-0.270944436,0.02));
#9824=CARTESIAN_POINT('Origin',(0.505,-0.25,5.93275428784068E-18));
#9825=CARTESIAN_POINT('',(0.500000000000001,-0.25,-0.05));
#9826=CARTESIAN_POINT('',(0.510000000000001,-0.25,0.05));
#9827=CARTESIAN_POINT('Origin',(0.505,-0.3532736505,-0.05));
#9828=CARTESIAN_POINT('',(0.510000000000001,-0.456547301,-0.05));
#9829=CARTESIAN_POINT('Origin',(0.505,-0.456547301000001,5.93275428784068E-18));
#9830=CARTESIAN_POINT('',(0.510000000000001,-0.456547301000001,0.05));
#9831=CARTESIAN_POINT('Origin',(0.505,-0.3532736505,0.05));
#9832=CARTESIAN_POINT('',(0.,0.,0.));
#9833=CARTESIAN_POINT('Origin',(-0.00639999889435817,-1.33725586897056E-10,
-2.60202312123977E-18));
#9834=CARTESIAN_POINT('',(-0.00750000021337694,-2.62982038223811E-17,-0.0248999997701383));
#9835=CARTESIAN_POINT('',(-0.00750000021337694,-9.33158505355009E-18,0.0248999997701383));
#9836=CARTESIAN_POINT('Origin',(-0.00750000021337694,-1.38314833296201E-10,
-2.61316366403604E-18));
#9837=CARTESIAN_POINT('',(-0.00639999976976533,-1.58005919577827E-12,0.0260000002475909));
#9838=CARTESIAN_POINT('Origin',(-0.00639999889435817,-9.20581548326642E-13,
0.0248999989285722));
#9839=CARTESIAN_POINT('',(-0.00639999976976533,-3.35121902792442E-17,-0.0260000002475909));
#9840=CARTESIAN_POINT('Origin',(-0.00639999977013826,-1.33725590550843E-10,
-2.60202313010945E-18));
#9841=CARTESIAN_POINT('Origin',(-0.00639999889435817,-9.20629689158185E-13,
-0.0248999989285722));
#9842=CARTESIAN_POINT('Origin',(-0.00639999889435817,1.33725588194013E-10,
-2.25687613815873E-19));
#9843=CARTESIAN_POINT('Origin',(-0.00750000021337694,1.38314834487708E-10,
-2.3310041583336E-19));
#9844=CARTESIAN_POINT('Origin',(-0.00639999977013826,1.3372558821988E-10,
4.44089209850063E-18));
#9845=CARTESIAN_POINT('Origin',(-0.0206375,0.,-4.33144407778805E-52));
#9846=CARTESIAN_POINT('',(0.00639999998722997,-6.70342338705283E-12,0.0260000000825303));
#9847=CARTESIAN_POINT('',(0.00639999998722997,-5.37097589710219E-12,-0.0260000000825303));
#9848=CARTESIAN_POINT('Origin',(0.0064,0.,-9.01972807340825E-19));
#9849=CARTESIAN_POINT('Origin',(0.0064,2.91826343292479E-18,0.));
#9850=CARTESIAN_POINT('',(-0.0206375,-3.18408167778312E-18,0.026));
#9851=CARTESIAN_POINT('Origin',(-0.0075,-1.31838984174237E-18,-1.2490009027033E-18));
#9852=CARTESIAN_POINT('',(-0.0075,-2.50440270425634E-18,0.02045));
#9853=CARTESIAN_POINT('Origin',(-0.0075,0.,0.));
#9854=CARTESIAN_POINT('Origin',(0.00639999889435816,-1.33725593635445E-10,
-3.59711256079879E-19));
#9855=CARTESIAN_POINT('',(0.00750000021337694,-1.05191955076574E-17,0.0248999997701383));
#9856=CARTESIAN_POINT('Origin',(0.00639999889435816,-9.20588335445364E-13,
0.0248999989285722));
#9857=CARTESIAN_POINT('',(0.00750000021337694,-2.93287844693988E-17,-0.0248999997701383));
#9858=CARTESIAN_POINT('Origin',(0.00750000021337694,-1.38314840140043E-10,
-3.71488919652902E-19));
#9859=CARTESIAN_POINT('Origin',(0.00639999889435816,-9.20608946339399E-13,
-0.0248999989285722));
#9860=CARTESIAN_POINT('Origin',(-0.0206375,0.,0.));
#9861=CARTESIAN_POINT('',(-0.00413672599961696,1.0458235455062E-18,0.0204500000364447));
#9862=CARTESIAN_POINT('',(-0.0206375,-2.50440270425634E-18,0.02045));
#9863=CARTESIAN_POINT('',(-0.004136726,-0.02045,-2.79956704802153E-18));
#9864=CARTESIAN_POINT('Origin',(-0.004136726,1.15025496390116E-19,8.88178419700125E-18));
#9865=CARTESIAN_POINT('Origin',(-0.004136726,1.15025496390116E-19,8.88178419700125E-18));
#9866=CARTESIAN_POINT('Origin',(0.00639999889435816,1.33725592594967E-10,
2.43522299685913E-19));
#9867=CARTESIAN_POINT('Origin',(0.00750000021337694,1.3831483908365E-10,
2.45725725091783E-19));
#9868=CARTESIAN_POINT('Origin',(0.0075,-1.31838984174237E-18,1.2490009027033E-18));
#9869=CARTESIAN_POINT('',(0.0075,-2.50440270425634E-18,0.02045));
#9870=CARTESIAN_POINT('Origin',(0.0075,0.,0.));
#9871=CARTESIAN_POINT('Origin',(4.25120033285821E-10,2.32696931299848E-18,
-2.53637255105429E-19));
#9872=CARTESIAN_POINT('',(-0.00413672599923392,-0.0130499999271107,-1.89332840771843E-18));
#9873=CARTESIAN_POINT('Origin',(4.25120034352053E-10,-0.01675,-2.30492064367725E-18));
#9874=CARTESIAN_POINT('',(-0.00413672599923392,-9.72427111671565E-12,0.0130499999635554));
#9875=CARTESIAN_POINT('Origin',(-0.00413672599923392,-2.48296911984889E-18,
-8.56610574398074E-20));
#9876=CARTESIAN_POINT('Origin',(-0.00413672599923392,-2.48296911984889E-18,
-8.56610574398074E-20));
#9877=CARTESIAN_POINT('Origin',(-0.0206375,0.,0.));
#9878=CARTESIAN_POINT('',(0.004136726,-0.02045,-1.97855791081413E-18));
#9879=CARTESIAN_POINT('',(0.004136726,-2.50440270425634E-18,0.02045));
#9880=CARTESIAN_POINT('Origin',(0.004136726,-1.49874617044541E-18,-8.88178419700125E-18));
#9881=CARTESIAN_POINT('Origin',(0.004136726,-1.49874617044541E-18,-8.88178419700125E-18));
#9882=CARTESIAN_POINT('',(-0.0206375,-2.50440270425634E-18,0.02045));
#9883=CARTESIAN_POINT('Origin',(-0.0206375,0.,0.));
#9884=CARTESIAN_POINT('',(-0.0075,-1.5981640728873E-18,0.01305));
#9885=CARTESIAN_POINT('',(-0.0206375,-1.5981640728873E-18,0.01305));
#9886=CARTESIAN_POINT('Origin',(-0.0075,0.,0.));
#9887=CARTESIAN_POINT('Origin',(-4.25120036303284E-10,3.75386134271222E-18,
6.07632462000188E-19));
#9888=CARTESIAN_POINT('',(0.00413672599923392,-2.67659699192252E-12,0.0130499999635553));
#9889=CARTESIAN_POINT('',(0.00413672599923392,-0.01305,-1.07231927942994E-18));
#9890=CARTESIAN_POINT('Origin',(0.00413672599923392,-3.3221160294436E-19,
2.22044604925031E-18));
#9891=CARTESIAN_POINT('Origin',(-4.25120034317525E-10,-0.01675,-1.44365092657163E-18));
#9892=CARTESIAN_POINT('Origin',(0.00413672599923392,-3.3221160294436E-19,
2.22044604925031E-18));
#9893=CARTESIAN_POINT('Origin',(-0.0075,-1.3010426069826E-19,-1.1666015375944E-18));
#9894=CARTESIAN_POINT('',(-0.00750000021337695,-7.32444758467801E-18,-0.00860000022986174));
#9895=CARTESIAN_POINT('',(-0.00750000021337695,-9.55563692214474E-13,0.00860000022983698));
#9896=CARTESIAN_POINT('Origin',(-0.00750000021337695,1.20438122996688E-10,
1.91155415755433E-19));
#9897=CARTESIAN_POINT('Origin',(-0.00750000021337695,-1.20438124044286E-10,
-1.263242268E-19));
#9898=CARTESIAN_POINT('Origin',(-0.0206375,0.,0.));
#9899=CARTESIAN_POINT('',(0.0075,-1.5981640728873E-18,0.01305));
#9900=CARTESIAN_POINT('Origin',(0.0075,0.,0.));
#9901=CARTESIAN_POINT('',(-0.0206375,-1.5981640728873E-18,0.01305));
#9902=CARTESIAN_POINT('Origin',(-0.00639999889435815,-1.33725589876008E-10,
-1.99489279445979E-19));
#9903=CARTESIAN_POINT('',(-0.00639999933187528,-1.78004529143068E-13,0.00749999975240887));
#9904=CARTESIAN_POINT('Origin',(-0.00639999889435815,-4.29138899262724E-13,
0.00860000107142784));
#9905=CARTESIAN_POINT('',(-0.00639999933187528,7.82593383085413E-14,-0.00749999975240887));
#9906=CARTESIAN_POINT('Origin',(-0.00639999977013826,-1.33725577217623E-10,
-2.22044604925031E-18));
#9907=CARTESIAN_POINT('Origin',(-0.00639999889435815,-4.29112928832131E-13,
-0.00860000107142784));
#9908=CARTESIAN_POINT('Origin',(-0.00639999889435816,1.33725589406987E-10,
2.62934110861178E-19));
#9909=CARTESIAN_POINT('Origin',(-0.00639999889435816,1.33725589406987E-10,
2.62934110861178E-19));
#9910=CARTESIAN_POINT('Origin',(0.0075,-1.3010426069826E-19,1.1666015375944E-18));
#9911=CARTESIAN_POINT('',(0.00750000021337695,-1.12844211802569E-18,0.00860000022986174));
#9912=CARTESIAN_POINT('',(0.00750000021337695,-9.55567354576375E-13,-0.00860000022983698));
#9913=CARTESIAN_POINT('Origin',(0.00750000021337695,1.20438122943562E-10,
-1.36910420000699E-19));
#9914=CARTESIAN_POINT('Origin',(0.00750000021337695,-1.20438123513651E-10,
2.9038238015475E-19));
#9915=CARTESIAN_POINT('Origin',(-0.0206375,0.,-2.49552314011156E-51));
#9916=CARTESIAN_POINT('',(0.00639999944717908,-3.41326938021997E-12,0.00749999987620436));
#9917=CARTESIAN_POINT('',(-0.0206375,-9.18485099360515E-19,0.0075));
#9918=CARTESIAN_POINT('',(0.00639999944670613,1.23481356905966E-13,-0.0074999998349392));
#9919=CARTESIAN_POINT('Origin',(0.0064,-1.93061231994698E-18,-5.55111512312578E-18));
#9920=CARTESIAN_POINT('Origin',(0.00639999889435815,1.33725588774518E-10,
-1.62015184442301E-19));
#9921=CARTESIAN_POINT('Origin',(0.00639999889435815,-1.33725589355705E-10,
3.07932432666985E-19));
#9922=CARTESIAN_POINT('Origin',(0.00639999889435815,-4.29128599184298E-13,
0.00860000107142785));
#9923=CARTESIAN_POINT('Origin',(0.00639999889435815,-4.2911240869608E-13,
-0.00860000107142785));
#9924=CARTESIAN_POINT('Origin',(0.00639999889435815,1.33725588774518E-10,
-1.62015184442301E-19));
#9925=CARTESIAN_POINT('',(0.,0.,0.));
#9926=CARTESIAN_POINT('Origin',(-0.46,0.35,-1.1));
#9927=CARTESIAN_POINT('',(-0.5,0.35,-1.128));
#9928=CARTESIAN_POINT('Origin',(-0.5,0.35,-1.1));
#9929=CARTESIAN_POINT('',(-0.46,0.35,-1.128));
#9930=CARTESIAN_POINT('',(-0.46,0.35,-1.128));
#9931=CARTESIAN_POINT('Origin',(-0.46,0.35,-1.1));
#9932=CARTESIAN_POINT('Origin',(-0.46,0.35,-1.1));
#9933=CARTESIAN_POINT('',(-0.46,0.35,-1.075));
#9934=CARTESIAN_POINT('Origin',(-0.46,0.35,-1.1));
#9935=CARTESIAN_POINT('Origin',(-0.5,0.35003431001795,-1.0350379192153));
#9936=CARTESIAN_POINT('',(-0.500000000000482,0.35,-0.920000000000262));
#9937=CARTESIAN_POINT('',(-0.500000000000482,0.392836676218822,-1.07421203438571));
#9938=CARTESIAN_POINT('Origin',(-0.5,0.649,-0.92));
#9939=CARTESIAN_POINT('',(-0.5,0.3,-0.92));
#9940=CARTESIAN_POINT('',(-0.5,0.3,-0.92));
#9941=CARTESIAN_POINT('',(-0.5,0.3,-1.09999999999836));
#9942=CARTESIAN_POINT('',(-0.5,0.3,-1.09999999952063));
#9943=CARTESIAN_POINT('Origin',(-0.5,0.35,-1.1));
#9944=CARTESIAN_POINT('',(-0.5,0.3125,-0.975));
#9945=CARTESIAN_POINT('Origin',(-0.5,0.3125,-0.98));
#9946=CARTESIAN_POINT('',(-0.5,0.3375,-0.935));
#9947=CARTESIAN_POINT('Origin',(-0.5,0.3375,-0.94));
#9948=CARTESIAN_POINT('',(-0.5,0.3375,-0.975));
#9949=CARTESIAN_POINT('Origin',(-0.5,0.3375,-0.98));
#9950=CARTESIAN_POINT('',(-0.5,0.3125,-0.935));
#9951=CARTESIAN_POINT('Origin',(-0.5,0.3125,-0.94));
#9952=CARTESIAN_POINT('Origin',(-0.51,0.35,-1.1));
#9953=CARTESIAN_POINT('',(-0.51,0.35,-1.075));
#9954=CARTESIAN_POINT('Origin',(-0.51,0.35,-1.1));
#9955=CARTESIAN_POINT('',(-0.51,0.35,-1.075));
#9956=CARTESIAN_POINT('Origin',(-0.51,0.3125,-0.94));
#9957=CARTESIAN_POINT('',(-0.51,0.3125,-0.935));
#9958=CARTESIAN_POINT('Origin',(-0.51,0.3125,-0.94));
#9959=CARTESIAN_POINT('',(-0.51,0.3125,-0.935));
#9960=CARTESIAN_POINT('Origin',(-0.51,0.3375,-0.98));
#9961=CARTESIAN_POINT('',(-0.51,0.3375,-0.975));
#9962=CARTESIAN_POINT('Origin',(-0.51,0.3375,-0.98));
#9963=CARTESIAN_POINT('',(-0.51,0.3375,-0.975));
#9964=CARTESIAN_POINT('Origin',(-0.51,0.3375,-0.94));
#9965=CARTESIAN_POINT('',(-0.51,0.3375,-0.935));
#9966=CARTESIAN_POINT('Origin',(-0.51,0.3375,-0.94));
#9967=CARTESIAN_POINT('',(-0.51,0.3375,-0.935));
#9968=CARTESIAN_POINT('Origin',(-0.51,0.3125,-0.98));
#9969=CARTESIAN_POINT('',(-0.51,0.3125,-0.975));
#9970=CARTESIAN_POINT('Origin',(-0.51,0.3125,-0.98));
#9971=CARTESIAN_POINT('',(-0.51,0.3125,-0.975));
#9972=CARTESIAN_POINT('Origin',(-0.505,0.325,-0.92));
#9973=CARTESIAN_POINT('',(-0.51,0.3,-0.92));
#9974=CARTESIAN_POINT('',(-0.500000000000001,0.3,-0.92));
#9975=CARTESIAN_POINT('',(-0.509999999999358,0.35,-0.92));
#9976=CARTESIAN_POINT('',(-0.50999999975,0.35,-0.92));
#9977=CARTESIAN_POINT('',(-0.510000000000001,0.3,-0.92));
#9978=CARTESIAN_POINT('Origin',(-0.505,0.3,-1.01));
#9979=CARTESIAN_POINT('',(-0.51,0.3,-1.09999999999807));
#9980=CARTESIAN_POINT('',(-0.510000000000001,0.3,-0.920000000000001));
#9981=CARTESIAN_POINT('',(-0.510000000000001,0.3,-1.1));
#9982=CARTESIAN_POINT('Origin',(-0.51,0.35,-1.1));
#9983=CARTESIAN_POINT('',(-0.51,0.39283667622015,-1.07421203438792));
#9984=CARTESIAN_POINT('',(-0.50000000025,0.392836676219352,-1.07421203438659));
#9985=CARTESIAN_POINT('Origin',(-0.51,0.35,-1.1));
#9986=CARTESIAN_POINT('Origin',(-0.51,0.649,-0.92));
#9987=CARTESIAN_POINT('Origin',(-0.51,0.649,-0.92));
#9988=CARTESIAN_POINT('Origin',(-0.51,0.35003431001795,-1.0350379192153));
#9989=CARTESIAN_POINT('',(0.,0.,0.));
#9990=CARTESIAN_POINT('Origin',(-0.00639999889435817,-1.33725586897056E-10,
-2.60202312123977E-18));
#9991=CARTESIAN_POINT('',(-0.00750000021337694,-2.62982038223811E-17,-0.0248999997701383));
#9992=CARTESIAN_POINT('',(-0.00750000021337694,-9.33158505355009E-18,0.0248999997701383));
#9993=CARTESIAN_POINT('Origin',(-0.00750000021337694,-1.38314833296201E-10,
-2.61316366403604E-18));
#9994=CARTESIAN_POINT('',(-0.00639999976976533,-1.58005919577827E-12,0.0260000002475909));
#9995=CARTESIAN_POINT('Origin',(-0.00639999889435817,-9.20581548326642E-13,
0.0248999989285722));
#9996=CARTESIAN_POINT('',(-0.00639999976976533,-3.35121902792442E-17,-0.0260000002475909));
#9997=CARTESIAN_POINT('Origin',(-0.00639999977013826,-1.33725590550843E-10,
-2.60202313010945E-18));
#9998=CARTESIAN_POINT('Origin',(-0.00639999889435817,-9.20629689158185E-13,
-0.0248999989285722));
#9999=CARTESIAN_POINT('Origin',(-0.00639999889435817,1.33725588194013E-10,
-2.25687613815873E-19));
#10000=CARTESIAN_POINT('Origin',(-0.00750000021337694,1.38314834487708E-10,
-2.3310041583336E-19));
#10001=CARTESIAN_POINT('Origin',(-0.00639999977013826,1.3372558821988E-10,
4.44089209850063E-18));
#10002=CARTESIAN_POINT('Origin',(-0.0206375,0.,-4.33144407778805E-52));
#10003=CARTESIAN_POINT('',(0.00639999998722997,-6.70342338705283E-12,0.0260000000825303));
#10004=CARTESIAN_POINT('',(0.00639999998722997,-5.37097589710219E-12,-0.0260000000825303));
#10005=CARTESIAN_POINT('Origin',(0.0064,0.,-9.01972807340825E-19));
#10006=CARTESIAN_POINT('Origin',(0.0064,2.91826343292479E-18,0.));
#10007=CARTESIAN_POINT('',(-0.0206375,-3.18408167778312E-18,0.026));
#10008=CARTESIAN_POINT('Origin',(-0.0075,-1.31838984174237E-18,-1.2490009027033E-18));
#10009=CARTESIAN_POINT('',(-0.0075,-2.50440270425634E-18,0.02045));
#10010=CARTESIAN_POINT('Origin',(-0.0075,0.,0.));
#10011=CARTESIAN_POINT('Origin',(0.00639999889435816,-1.33725593635445E-10,
-3.59711256079879E-19));
#10012=CARTESIAN_POINT('',(0.00750000021337694,-1.05191955076574E-17,0.0248999997701383));
#10013=CARTESIAN_POINT('Origin',(0.00639999889435816,-9.20588335445364E-13,
0.0248999989285722));
#10014=CARTESIAN_POINT('',(0.00750000021337694,-2.93287844693988E-17,-0.0248999997701383));
#10015=CARTESIAN_POINT('Origin',(0.00750000021337694,-1.38314840140043E-10,
-3.71488919652902E-19));
#10016=CARTESIAN_POINT('Origin',(0.00639999889435816,-9.20608946339399E-13,
-0.0248999989285722));
#10017=CARTESIAN_POINT('Origin',(-0.0206375,0.,0.));
#10018=CARTESIAN_POINT('',(-0.00413672599961696,1.0458235455062E-18,0.0204500000364447));
#10019=CARTESIAN_POINT('',(-0.0206375,-2.50440270425634E-18,0.02045));
#10020=CARTESIAN_POINT('',(-0.004136726,-0.02045,-2.79956704802153E-18));
#10021=CARTESIAN_POINT('Origin',(-0.004136726,1.15025496390116E-19,8.88178419700125E-18));
#10022=CARTESIAN_POINT('Origin',(-0.004136726,1.15025496390116E-19,8.88178419700125E-18));
#10023=CARTESIAN_POINT('Origin',(0.00639999889435816,1.33725592594967E-10,
2.43522299685913E-19));
#10024=CARTESIAN_POINT('Origin',(0.00750000021337694,1.3831483908365E-10,
2.45725725091783E-19));
#10025=CARTESIAN_POINT('Origin',(0.0075,-1.31838984174237E-18,1.2490009027033E-18));
#10026=CARTESIAN_POINT('',(0.0075,-2.50440270425634E-18,0.02045));
#10027=CARTESIAN_POINT('Origin',(0.0075,0.,0.));
#10028=CARTESIAN_POINT('Origin',(4.25120033285821E-10,2.32696931299848E-18,
-2.53637255105429E-19));
#10029=CARTESIAN_POINT('',(-0.00413672599923392,-0.0130499999271107,-1.89332840771843E-18));
#10030=CARTESIAN_POINT('Origin',(4.25120034352053E-10,-0.01675,-2.30492064367725E-18));
#10031=CARTESIAN_POINT('',(-0.00413672599923392,-9.72427111671565E-12,0.0130499999635554));
#10032=CARTESIAN_POINT('Origin',(-0.00413672599923392,-2.48296911984889E-18,
-8.56610574398074E-20));
#10033=CARTESIAN_POINT('Origin',(-0.00413672599923392,-2.48296911984889E-18,
-8.56610574398074E-20));
#10034=CARTESIAN_POINT('Origin',(-0.0206375,0.,0.));
#10035=CARTESIAN_POINT('',(0.004136726,-0.02045,-1.97855791081413E-18));
#10036=CARTESIAN_POINT('',(0.004136726,-2.50440270425634E-18,0.02045));
#10037=CARTESIAN_POINT('Origin',(0.004136726,-1.49874617044541E-18,-8.88178419700125E-18));
#10038=CARTESIAN_POINT('Origin',(0.004136726,-1.49874617044541E-18,-8.88178419700125E-18));
#10039=CARTESIAN_POINT('',(-0.0206375,-2.50440270425634E-18,0.02045));
#10040=CARTESIAN_POINT('Origin',(-0.0206375,0.,0.));
#10041=CARTESIAN_POINT('',(-0.0075,-1.5981640728873E-18,0.01305));
#10042=CARTESIAN_POINT('',(-0.0206375,-1.5981640728873E-18,0.01305));
#10043=CARTESIAN_POINT('Origin',(-0.0075,0.,0.));
#10044=CARTESIAN_POINT('Origin',(-4.25120036303284E-10,3.75386134271222E-18,
6.07632462000188E-19));
#10045=CARTESIAN_POINT('',(0.00413672599923392,-2.67659699192252E-12,0.0130499999635553));
#10046=CARTESIAN_POINT('',(0.00413672599923392,-0.01305,-1.07231927942994E-18));
#10047=CARTESIAN_POINT('Origin',(0.00413672599923392,-3.3221160294436E-19,
2.22044604925031E-18));
#10048=CARTESIAN_POINT('Origin',(-4.25120034317525E-10,-0.01675,-1.44365092657163E-18));
#10049=CARTESIAN_POINT('Origin',(0.00413672599923392,-3.3221160294436E-19,
2.22044604925031E-18));
#10050=CARTESIAN_POINT('Origin',(-0.0075,-1.3010426069826E-19,-1.1666015375944E-18));
#10051=CARTESIAN_POINT('',(-0.00750000021337695,-7.32444758467801E-18,-0.00860000022986174));
#10052=CARTESIAN_POINT('',(-0.00750000021337695,-9.55563692214474E-13,0.00860000022983698));
#10053=CARTESIAN_POINT('Origin',(-0.00750000021337695,1.20438122996688E-10,
1.91155415755433E-19));
#10054=CARTESIAN_POINT('Origin',(-0.00750000021337695,-1.20438124044286E-10,
-1.263242268E-19));
#10055=CARTESIAN_POINT('Origin',(-0.0206375,0.,0.));
#10056=CARTESIAN_POINT('',(0.0075,-1.5981640728873E-18,0.01305));
#10057=CARTESIAN_POINT('Origin',(0.0075,0.,0.));
#10058=CARTESIAN_POINT('',(-0.0206375,-1.5981640728873E-18,0.01305));
#10059=CARTESIAN_POINT('Origin',(-0.00639999889435815,-1.33725589876008E-10,
-1.99489279445979E-19));
#10060=CARTESIAN_POINT('',(-0.00639999933187528,-1.78004529143068E-13,0.00749999975240887));
#10061=CARTESIAN_POINT('Origin',(-0.00639999889435815,-4.29138899262724E-13,
0.00860000107142784));
#10062=CARTESIAN_POINT('',(-0.00639999933187528,7.82593383085413E-14,-0.00749999975240887));
#10063=CARTESIAN_POINT('Origin',(-0.00639999977013826,-1.33725577217623E-10,
-2.22044604925031E-18));
#10064=CARTESIAN_POINT('Origin',(-0.00639999889435815,-4.29112928832131E-13,
-0.00860000107142784));
#10065=CARTESIAN_POINT('Origin',(-0.00639999889435816,1.33725589406987E-10,
2.62934110861178E-19));
#10066=CARTESIAN_POINT('Origin',(-0.00639999889435816,1.33725589406987E-10,
2.62934110861178E-19));
#10067=CARTESIAN_POINT('Origin',(0.0075,-1.3010426069826E-19,1.1666015375944E-18));
#10068=CARTESIAN_POINT('',(0.00750000021337695,-1.12844211802569E-18,0.00860000022986174));
#10069=CARTESIAN_POINT('',(0.00750000021337695,-9.55567354576375E-13,-0.00860000022983698));
#10070=CARTESIAN_POINT('Origin',(0.00750000021337695,1.20438122943562E-10,
-1.36910420000699E-19));
#10071=CARTESIAN_POINT('Origin',(0.00750000021337695,-1.20438123513651E-10,
2.9038238015475E-19));
#10072=CARTESIAN_POINT('Origin',(-0.0206375,0.,-2.49552314011156E-51));
#10073=CARTESIAN_POINT('',(0.00639999944717908,-3.41326938021997E-12,0.00749999987620436));
#10074=CARTESIAN_POINT('',(-0.0206375,-9.18485099360515E-19,0.0075));
#10075=CARTESIAN_POINT('',(0.00639999944670613,1.23481356905966E-13,-0.0074999998349392));
#10076=CARTESIAN_POINT('Origin',(0.0064,-1.93061231994698E-18,-5.55111512312578E-18));
#10077=CARTESIAN_POINT('Origin',(0.00639999889435815,1.33725588774518E-10,
-1.62015184442301E-19));
#10078=CARTESIAN_POINT('Origin',(0.00639999889435815,-1.33725589355705E-10,
3.07932432666985E-19));
#10079=CARTESIAN_POINT('Origin',(0.00639999889435815,-4.29128599184298E-13,
0.00860000107142785));
#10080=CARTESIAN_POINT('Origin',(0.00639999889435815,-4.2911240869608E-13,
-0.00860000107142785));
#10081=CARTESIAN_POINT('Origin',(0.00639999889435815,1.33725588774518E-10,
-1.62015184442301E-19));
#10082=CARTESIAN_POINT('',(0.,0.,0.));
#10083=CARTESIAN_POINT('',(0.,0.,0.));
#10084=CARTESIAN_POINT('Origin',(0.,0.121795515,1.128682977));
#10085=CARTESIAN_POINT('',(-9.79717407256475E-19,0.120797846530031,1.12074542993335));
#10086=CARTESIAN_POINT('Origin',(0.,0.121795515265017,1.12868297696669));
#10087=CARTESIAN_POINT('',(-9.79717407256475E-19,0.347017944542894,1.09231187003569));
#10088=CARTESIAN_POINT('',(-9.79717407256475E-19,0.120797846265014,1.12074542996666));
#10089=CARTESIAN_POINT('Origin',(0.,0.34801561327788,1.10024941706903));
#10090=CARTESIAN_POINT('Origin',(-1.99493199737333E-19,0.348015613,1.100249417));
#10091=CARTESIAN_POINT('Origin',(-1.56125112837913E-19,0.121795515,1.128682977));
#10092=CARTESIAN_POINT('',(-1.22464678562706E-18,0.120548429108451,1.11876104298636));
#10093=CARTESIAN_POINT('Origin',(0.,0.121795515054226,1.12868297699318));
#10094=CARTESIAN_POINT('Origin',(0.,0.121795515,1.128682977));
#10095=CARTESIAN_POINT('',(-1.22464678562706E-18,0.34875291409482,1.09007806587791));
#10096=CARTESIAN_POINT('Origin',(0.,0.350000000040595,1.09999999988473));
#10097=CARTESIAN_POINT('',(-1.22464678562706E-18,0.120548429054225,1.11876104299317));
#10098=CARTESIAN_POINT('Origin',(-1.56125112837913E-19,0.35,1.1));
#10099=CARTESIAN_POINT('',(0.,0.,0.));
#10100=CARTESIAN_POINT('Origin',(0.,0.305351296,1.105611887));
#10101=CARTESIAN_POINT('',(0.00278388211169927,-0.147032020331956,1.15491284800427));
#10102=CARTESIAN_POINT('',(-0.00278388211169927,-0.147032020331956,1.15491284800427));
#10103=CARTESIAN_POINT('Origin',(0.,-0.146096706241833,1.16235429820977));
#10104=CARTESIAN_POINT('',(-0.00800000000069301,-0.14609670602179,1.16235429794207));
#10105=CARTESIAN_POINT('Origin',(0.,-0.146096706241833,1.16235429820977));
#10106=CARTESIAN_POINT('',(-0.0027838802685275,-0.145161391367063,1.16979574904614));
#10107=CARTESIAN_POINT('Origin',(0.,-0.146096706241833,1.16235429820977));
#10108=CARTESIAN_POINT('',(-9.79717391973985E-19,-0.14509903752142,1.17029184511916));
#10109=CARTESIAN_POINT('Origin',(0.,-0.146096706241833,1.16235429820977));
#10110=CARTESIAN_POINT('',(-9.79717391973985E-19,0.306348965440833,1.11354943381884));
#10111=CARTESIAN_POINT('',(-9.79717391973985E-19,0.306348964720413,1.11354943390939));
#10112=CARTESIAN_POINT('Origin',(0.,0.30535129672042,1.10561188690945));
#10113=CARTESIAN_POINT('',(0.00278388026853193,-0.145161391367063,1.16979574904614));
#10114=CARTESIAN_POINT('Origin',(0.,-0.146096706241833,1.16235429820977));
#10115=CARTESIAN_POINT('',(0.00800000000069306,-0.146096706021879,1.16235429794136));
#10116=CARTESIAN_POINT('Origin',(0.,-0.146096706241833,1.16235429820977));
#10117=CARTESIAN_POINT('Origin',(0.,-0.146096706241833,1.16235429820977));
#10118=CARTESIAN_POINT('Origin',(-1.99493199737333E-19,0.3053512965,1.105611887));
#10119=CARTESIAN_POINT('Origin',(-2.16840434497101E-21,-0.145130214061639,
1.17004379721066));
#10120=CARTESIAN_POINT('',(-0.00278388206046948,-0.145161391,1.169795749));
#10121=CARTESIAN_POINT('Origin',(0.0053919408556245,-0.145629048554537,
1.16607502335495));
#10122=CARTESIAN_POINT('',(0.00800000019173051,-0.145161390945555,1.16979574899316));
#10123=CARTESIAN_POINT('',(0.0080000001755413,-0.145161390894627,1.16979574898676));
#10124=CARTESIAN_POINT('',(0.00278388206046948,-0.145161391,1.169795749));
#10125=CARTESIAN_POINT('Origin',(0.0053919408556245,-0.146564362942481,
1.15863357314803));
#10126=CARTESIAN_POINT('',(0.00800000023881122,-0.147032019932316,1.15491284799148));
#10127=CARTESIAN_POINT('',(0.008,-0.14703202,1.154912848));
#10128=CARTESIAN_POINT('',(0.00800000035492486,-0.146096705717927,1.16235429790316));
#10129=CARTESIAN_POINT('Origin',(-2.16840434497101E-21,-0.147063197435379,
1.15466479929232));
#10130=CARTESIAN_POINT('',(0.00278388206047103,-0.14703202,1.154912848));
#10131=CARTESIAN_POINT('Origin',(-0.00539194085562444,-0.146564362942481,
1.15863357314803));
#10132=CARTESIAN_POINT('',(-0.00800000023876324,-0.147032019932289,1.15491284799148));
#10133=CARTESIAN_POINT('',(-0.00800000021850583,-0.147032019868836,1.15491284798351));
#10134=CARTESIAN_POINT('',(-0.00278388206047102,-0.14703202,1.154912848));
#10135=CARTESIAN_POINT('Origin',(-0.00539194085562444,-0.145629048554537,
1.16607502335495));
#10136=CARTESIAN_POINT('',(-0.00800000019173049,-0.145161390945555,1.16979574899316));
#10137=CARTESIAN_POINT('',(-0.00799999999999999,-0.145161391,1.169795749));
#10138=CARTESIAN_POINT('',(-0.00800000042103161,-0.146096705826252,1.16235429791749));
#10139=CARTESIAN_POINT('Origin',(-8.88178419700125E-18,-0.3436000735,1.194737468));
#10140=CARTESIAN_POINT('',(-0.249999999778211,-0.542038756006933,1.21967918700087));
#10141=CARTESIAN_POINT('',(-0.2499999997114,-0.542038755954343,1.21967918699426));
#10142=CARTESIAN_POINT('',(0.249999999778211,-0.542038756006933,1.21967918700087));
#10143=CARTESIAN_POINT('',(0.249999999800629,-0.542038756,1.219679187));
#10144=CARTESIAN_POINT('',(0.00800000019883055,-0.145161390932821,1.16979574899156));
#10145=CARTESIAN_POINT('Origin',(0.129,-0.344535388,1.18729601725));
#10146=CARTESIAN_POINT('',(0.249999999858746,-0.543909385010705,1.20479628600136));
#10147=CARTESIAN_POINT('',(0.249999999902924,-0.543909384930022,1.20479628655675));
#10148=CARTESIAN_POINT('',(0.00800000026765782,-0.147032019949447,1.15491284799364));
#10149=CARTESIAN_POINT('Origin',(-8.88178419700125E-18,-0.3454707025,1.17985456699999));
#10150=CARTESIAN_POINT('',(-0.249999999858735,-0.543909385010698,1.20479628600136));
#10151=CARTESIAN_POINT('',(0.249999999800629,-0.543909385000001,1.20479628599999));
#10152=CARTESIAN_POINT('',(-0.249999999754365,-0.543909384928553,1.20479628599101));
#10153=CARTESIAN_POINT('Origin',(-0.129,-0.344535388,1.18729601725));
#10154=CARTESIAN_POINT('',(-0.249999999902924,-0.543909384930022,1.20479628655675));
#10155=CARTESIAN_POINT('Origin',(-8.88178419700125E-18,-0.5429740705,1.2122377365));
#10156=CARTESIAN_POINT('',(0.,0.,0.));
#10157=CARTESIAN_POINT('Origin',(0.,0.439262055,0.88802763));
#10158=CARTESIAN_POINT('',(-9.79717389180519E-19,0.446635006554106,0.891132397113708));
#10159=CARTESIAN_POINT('Origin',(0.,0.439262054946085,0.888027630128034));
#10160=CARTESIAN_POINT('',(-9.79717389180519E-19,0.358149142877981,1.10126152882899));
#10161=CARTESIAN_POINT('',(-9.79717389180519E-19,0.446635006608021,0.891132396985674));
#10162=CARTESIAN_POINT('Origin',(0.,0.350776191269958,1.09815676184331));
#10163=CARTESIAN_POINT('Origin',(-1.99493199737333E-19,0.3507761915,1.098156762));
#10164=CARTESIAN_POINT('Origin',(-1.56125112837913E-19,0.439262055499997,
0.888027630499999));
#10165=CARTESIAN_POINT('',(-1.22464675698891E-18,0.44847824432875,0.891908589594178));
#10166=CARTESIAN_POINT('Origin',(0.,0.439262054664349,0.888027630797078));
#10167=CARTESIAN_POINT('Origin',(0.,0.439262055,0.88802763));
#10168=CARTESIAN_POINT('',(-1.22464675698891E-18,0.359216189190635,1.10388095853602));
#10169=CARTESIAN_POINT('Origin',(0.,0.349999999526235,1.09999999973892));
#10170=CARTESIAN_POINT('',(-1.22464675698891E-18,0.448478244664401,0.891908588797101));
#10171=CARTESIAN_POINT('Origin',(-1.56125112837913E-19,0.35,1.1));
#10172=CARTESIAN_POINT('',(0.,0.,0.));
#10173=CARTESIAN_POINT('Origin',(0.,0.377184388,1.135860968));
#10174=CARTESIAN_POINT('',(0.00278388195593357,0.64607193114008,1.50298593209025));
#10175=CARTESIAN_POINT('',(-0.00278388195593361,0.64607193114008,1.50298593209025));
#10176=CARTESIAN_POINT('Origin',(0.,0.652048759141067,1.4984552009048));
#10177=CARTESIAN_POINT('',(-0.00799999980513634,0.652048759131474,1.49845520070589));
#10178=CARTESIAN_POINT('Origin',(0.,0.652048759141067,1.4984552009048));
#10179=CARTESIAN_POINT('',(-0.00278388142421084,0.658025587080488,1.49392446925429));
#10180=CARTESIAN_POINT('Origin',(0.,0.652048759141067,1.4984552009048));
#10181=CARTESIAN_POINT('',(-9.79717407621583E-19,0.658424042146736,1.49362242091224));
#10182=CARTESIAN_POINT('Origin',(0.,0.652048759141067,1.4984552009048));
#10183=CARTESIAN_POINT('',(-9.79717407621583E-19,0.383559671011319,1.13102818801489));
#10184=CARTESIAN_POINT('',(-9.79717407621583E-19,0.383559671005671,1.13102818800744));
#10185=CARTESIAN_POINT('Origin',(0.,0.377184388005651,1.13586096800745));
#10186=CARTESIAN_POINT('',(0.00278388142421076,0.658025587080488,1.49392446925429));
#10187=CARTESIAN_POINT('Origin',(0.,0.652048759141067,1.4984552009048));
#10188=CARTESIAN_POINT('',(0.00799999980513743,0.652048759130905,1.49845520070633));
#10189=CARTESIAN_POINT('Origin',(0.,0.652048759141067,1.4984552009048));
#10190=CARTESIAN_POINT('Origin',(0.,0.652048759141067,1.4984552009048));
#10191=CARTESIAN_POINT('Origin',(-1.99493199737333E-19,0.3771843885,1.1358609685));
#10192=CARTESIAN_POINT('Origin',(-2.16840434497101E-21,0.658224814634137,
1.49377344464617));
#10193=CARTESIAN_POINT('',(-0.00278388206047001,0.658025587,1.493924469));
#10194=CARTESIAN_POINT('Origin',(0.0053919408556245,0.655037172984959,1.49618983480451));
#10195=CARTESIAN_POINT('',(0.00799999981595462,0.658025587031806,1.49392446904196));
#10196=CARTESIAN_POINT('',(0.00799999983151832,0.658025587061577,1.49392446908123));
#10197=CARTESIAN_POINT('',(0.00278388206047,0.658025587,1.493924469));
#10198=CARTESIAN_POINT('Origin',(0.0053919408556245,0.64906034501504,1.50072056619548));
#10199=CARTESIAN_POINT('',(0.00799999989834483,0.64607193101772,1.50298593202338));
#10200=CARTESIAN_POINT('',(0.00800000000000001,0.646071930999999,1.502985932));
#10201=CARTESIAN_POINT('',(0.00799999983866159,0.65204875900126,1.49845520053531));
#10202=CARTESIAN_POINT('Origin',(-2.16840434497101E-21,0.645872703365862,
1.50313695635384));
#10203=CARTESIAN_POINT('',(0.00278388206047,0.646071930999999,1.502985932));
#10204=CARTESIAN_POINT('Origin',(-0.00539194085562444,0.64906034501504,
1.50072056619548));
#10205=CARTESIAN_POINT('',(-0.00799999989827039,0.646071931017694,1.50298593202334));
#10206=CARTESIAN_POINT('',(-0.00799999990666903,0.64607193103411,1.502985932045));
#10207=CARTESIAN_POINT('',(-0.00278388206047,0.646071930999999,1.502985932));
#10208=CARTESIAN_POINT('Origin',(-0.00539194085562444,0.655037172984959,
1.49618983480451));
#10209=CARTESIAN_POINT('',(-0.00799999981595463,0.658025587031806,1.49392446904196));
#10210=CARTESIAN_POINT('',(-0.00799999999999999,0.658025587,1.493924469));
#10211=CARTESIAN_POINT('',(-0.00799999989952599,0.652048759062608,1.49845520061504));
#10212=CARTESIAN_POINT('Origin',(-8.88178419700125E-18,0.778845090499999,
1.6533065495));
#10213=CARTESIAN_POINT('',(-0.249999999783566,0.899664593989047,1.81268862998555));
#10214=CARTESIAN_POINT('',(-0.249999999796965,0.899664593910672,1.81268862988216));
#10215=CARTESIAN_POINT('',(0.249999999783566,0.899664593989047,1.81268862998555));
#10216=CARTESIAN_POINT('',(0.249999999800629,0.899664593999999,1.81268863));
#10217=CARTESIAN_POINT('',(0.00799999985480845,0.658025587084829,1.49392446911191));
#10218=CARTESIAN_POINT('Origin',(0.129,0.772868262499999,1.65783728125));
#10219=CARTESIAN_POINT('',(0.249999999885983,0.88771093798903,1.82175009298553));
#10220=CARTESIAN_POINT('',(0.2499999998105,0.887710938334042,1.82175009274678));
#10221=CARTESIAN_POINT('',(0.00800000016977363,0.646071931296823,1.50298593239156));
#10222=CARTESIAN_POINT('Origin',(-8.88178419700125E-18,0.7668914345,1.6623680125));
#10223=CARTESIAN_POINT('',(-0.24999999988596,0.88771093798902,1.82175009298552));
#10224=CARTESIAN_POINT('',(0.249999999800629,0.887710938,1.821750093));
#10225=CARTESIAN_POINT('',(-0.24999999988113,0.887710937892202,1.8217500928578));
#10226=CARTESIAN_POINT('Origin',(-0.129,0.772868262499999,1.65783728125));
#10227=CARTESIAN_POINT('',(-0.2499999998105,0.887710938334042,1.82175009274678));
#10228=CARTESIAN_POINT('Origin',(-8.88178419700125E-18,0.893687766,1.8172193615));
#10229=CARTESIAN_POINT('',(0.,0.,0.));
#10230=CARTESIAN_POINT('Origin',(0.,0.367464315,1.058527145));
#10231=CARTESIAN_POINT('',(0.00278388280878993,0.550960089028251,0.64210121993291));
#10232=CARTESIAN_POINT('',(-0.00278388280878729,0.550960089028251,0.64210121993291));
#10233=CARTESIAN_POINT('Origin',(0.,0.544047946829229,0.63919050076935));
#10234=CARTESIAN_POINT('',(-0.00800000011528736,0.544047946993585,0.639190501008153));
#10235=CARTESIAN_POINT('Origin',(0.,0.544047946829229,0.63919050076935));
#10236=CARTESIAN_POINT('',(-0.00278388196528325,0.537135804154995,0.636279781774966));
#10237=CARTESIAN_POINT('Origin',(0.,0.544047946829229,0.63919050076935));
#10238=CARTESIAN_POINT('',(-9.79717434126005E-19,0.536674994885828,0.636085733634446));
#10239=CARTESIAN_POINT('Origin',(0.,0.544047946829229,0.63919050076935));
#10240=CARTESIAN_POINT('',(-9.79717434126005E-19,0.360091363113376,1.05542237773027));
#10241=CARTESIAN_POINT('',(-9.79717434126005E-19,0.360091363056599,1.0554223778651));
#10242=CARTESIAN_POINT('Origin',(0.,0.367464315056776,1.05852714486517));
#10243=CARTESIAN_POINT('',(0.00278388196528327,0.537135804154995,0.636279781774966));
#10244=CARTESIAN_POINT('Origin',(0.,0.544047946829229,0.63919050076935));
#10245=CARTESIAN_POINT('',(0.00800000011528736,0.544047946993585,0.639190501008153));
#10246=CARTESIAN_POINT('Origin',(0.,0.544047946829229,0.63919050076935));
#10247=CARTESIAN_POINT('Origin',(0.,0.544047946829229,0.63919050076935));
#10248=CARTESIAN_POINT('Origin',(-1.99493199737333E-19,0.3674643155,1.058527145));
#10249=CARTESIAN_POINT('Origin',(-2.16840434497101E-21,0.536905399427502,
0.636182758143169));
#10250=CARTESIAN_POINT('',(-0.00278388206046941,0.537135804,0.636279782));
#10251=CARTESIAN_POINT('Origin',(0.0053919408556245,0.540591875569578,0.637735141343516));
#10252=CARTESIAN_POINT('',(0.00800000011643423,0.537135803986997,0.636279782030879));
#10253=CARTESIAN_POINT('',(0.00800000010679859,0.537135803974924,0.636279782059549));
#10254=CARTESIAN_POINT('',(0.00278388206046941,0.537135804,0.636279782));
#10255=CARTESIAN_POINT('Origin',(0.0053919408556245,0.54750401792744,0.640645860656483));
#10256=CARTESIAN_POINT('',(0.00800000029334438,0.550960088967523,0.642101220077123));
#10257=CARTESIAN_POINT('',(0.00800000000000001,0.550960089,0.642101219999999));
#10258=CARTESIAN_POINT('',(0.0080000001207922,0.544047946835306,0.639190501384019));
#10259=CARTESIAN_POINT('Origin',(-2.16840434497101E-21,0.551190494069516,
0.642198243856831));
#10260=CARTESIAN_POINT('',(0.00278388206047068,0.550960089,0.64210122));
#10261=CARTESIAN_POINT('Origin',(-0.00539194085562444,0.54750401792744,
0.640645860656483));
#10262=CARTESIAN_POINT('',(-0.00800000029336689,0.550960088967528,0.642101220077111));
#10263=CARTESIAN_POINT('',(-0.00800000026828181,0.550960088937008,0.642101220149587));
#10264=CARTESIAN_POINT('',(-0.00278388206047068,0.550960089,0.642101219999999));
#10265=CARTESIAN_POINT('Origin',(-0.00539194085562444,0.540591875569578,
0.637735141343516));
#10266=CARTESIAN_POINT('',(-0.00800000011643421,0.537135803986997,0.636279782030879));
#10267=CARTESIAN_POINT('',(-0.00799999999999999,0.537135804,0.636279782));
#10268=CARTESIAN_POINT('',(-0.00800000042514707,0.544047947030544,0.639190500920384));
#10269=CARTESIAN_POINT('Origin',(-8.88178419700125E-18,0.614754983000001,
0.4519559825));
#10270=CARTESIAN_POINT('',(-0.249999999824503,0.69237416199696,0.267632183007222));
#10271=CARTESIAN_POINT('',(-0.249999999805892,0.692374161959955,0.267632183095097));
#10272=CARTESIAN_POINT('',(0.249999999824503,0.69237416199696,0.267632183007222));
#10273=CARTESIAN_POINT('',(0.249999999800628,0.692374162000001,0.267632183));
#10274=CARTESIAN_POINT('',(0.0080000001300884,0.537135803989865,0.636279782024071));
#10275=CARTESIAN_POINT('Origin',(0.129,0.621667125,0.4548667015));
#10276=CARTESIAN_POINT('',(0.249999999874932,0.706198446001423,0.273453620996678));
#10277=CARTESIAN_POINT('',(0.249999999890418,0.706198446007047,0.273453621002968));
#10278=CARTESIAN_POINT('',(0.00800000026828148,0.550960088937008,0.642101220149588));
#10279=CARTESIAN_POINT('Origin',(-8.88178419700125E-18,0.6285792675,0.457777420499999));
#10280=CARTESIAN_POINT('',(-0.249999999874803,0.706198446001377,0.273453620996738));
#10281=CARTESIAN_POINT('',(0.249999999800628,0.706198446,0.273453621));
#10282=CARTESIAN_POINT('',(-0.249999999795491,0.706198445962397,0.273453621089297));
#10283=CARTESIAN_POINT('Origin',(-0.129,0.621667125,0.4548667015));
#10284=CARTESIAN_POINT('',(-0.249999999890418,0.706198446007047,0.273453621002968));
#10285=CARTESIAN_POINT('Origin',(-8.88178419700125E-18,0.699286304,0.270542902));
#10286=CARTESIAN_POINT('',(0.,0.,0.));
#10287=CARTESIAN_POINT('Origin',(0.,0.488942429,1.283289392));
#10288=CARTESIAN_POINT('',(-9.79717407607493E-19,0.482567145986908,1.28812217198258));
#10289=CARTESIAN_POINT('Origin',(0.,0.488942428993417,1.28328939199132));
#10290=CARTESIAN_POINT('',(-9.79717407607493E-19,0.344832912126902,1.10642660087645));
#10291=CARTESIAN_POINT('',(-9.79717407607493E-19,0.482567145993489,1.28812217199126));
#10292=CARTESIAN_POINT('Origin',(0.,0.351208195133414,1.10159382088519));
#10293=CARTESIAN_POINT('Origin',(-1.99493199737333E-19,0.351208195,1.1015938205));
#10294=CARTESIAN_POINT('Origin',(-1.56125112837913E-19,0.488942429,1.2832893925));
#10295=CARTESIAN_POINT('',(-1.22464678389777E-18,0.480973325166166,1.28933036721888));
#10296=CARTESIAN_POINT('Origin',(0.,0.488942429083005,1.2832893921095));
#10297=CARTESIAN_POINT('Origin',(0.,0.488942429,1.283289392));
#10298=CARTESIAN_POINT('',(-1.22464678389777E-18,0.342030896187977,1.10604097520234));
#10299=CARTESIAN_POINT('Origin',(0.,0.350000000104818,1.10000000009296));
#10300=CARTESIAN_POINT('',(-1.22464678389777E-18,0.48097332508316,1.28933036710938));
#10301=CARTESIAN_POINT('Origin',(-1.56125112837913E-19,0.35,1.1));
#10302=CARTESIAN_POINT('',(0.,0.,0.));
#10303=CARTESIAN_POINT('Origin',(-0.459999999999996,0.350000000118451,1.09999999993794));
#10304=CARTESIAN_POINT('',(-0.473899999331871,0.346519549139845,1.09335647246591));
#10305=CARTESIAN_POINT('',(-0.473899999860731,0.353480450975115,1.10664352775337));
#10306=CARTESIAN_POINT('Origin',(-0.473899999770134,0.349999999881542,1.10000000006206));
#10307=CARTESIAN_POINT('',(-0.496099999999996,0.346519549379708,1.09335647234025));
#10308=CARTESIAN_POINT('',(-0.459999999999996,0.346519549379708,1.09335647234025));
#10309=CARTESIAN_POINT('',(-0.496100000552817,0.353480450914643,1.10664352764529));
#10310=CARTESIAN_POINT('Origin',(-0.496099999999996,0.349999999999997,1.1));
#10311=CARTESIAN_POINT('Origin',(-0.496099999999996,0.349999999999997,1.1));
#10312=CARTESIAN_POINT('Origin',(-0.473899999770134,0.349999999881542,1.10000000006206));
#10313=CARTESIAN_POINT('Origin',(-0.459999999999996,0.350000000118451,1.09999999993794));
#10314=CARTESIAN_POINT('',(-0.459999999999996,0.346519549379708,1.09335647234025));
#10315=CARTESIAN_POINT('Origin',(-0.459999999999996,0.350000000118451,1.09999999993794));
#10316=CARTESIAN_POINT('',(-0.461099999999996,0.346519549379708,1.09335647234025));
#10317=CARTESIAN_POINT('',(-0.459999999999996,0.346519549379708,1.09335647234025));
#10318=CARTESIAN_POINT('',(-0.461100000552817,0.353480450914643,1.10664352764529));
#10319=CARTESIAN_POINT('Origin',(-0.461099999999996,0.349999999999997,1.1));
#10320=CARTESIAN_POINT('Origin',(-0.461099999999996,0.349999999999997,1.1));
#10321=CARTESIAN_POINT('Origin',(-0.459999999999996,0.350000000118451,1.09999999993794));
#10322=CARTESIAN_POINT('',(-0.508899999331871,0.346519549139845,1.09335647246591));
#10323=CARTESIAN_POINT('',(-0.508899999860731,0.353480450975115,1.10664352775337));
#10324=CARTESIAN_POINT('Origin',(-0.508899999770134,0.349999999881542,1.10000000006206));
#10325=CARTESIAN_POINT('',(-0.61,0.346519549379708,1.09335647234025));
#10326=CARTESIAN_POINT('',(-0.459999999999996,0.346519549379708,1.09335647234025));
#10327=CARTESIAN_POINT('Origin',(-0.61,0.350000000118451,1.09999999993794));
#10328=CARTESIAN_POINT('Origin',(-0.508899999770134,0.349999999881542,1.10000000006206));
#10329=CARTESIAN_POINT('Origin',(0.46,0.350000000118451,1.09999999993794));
#10330=CARTESIAN_POINT('',(0.473899999447179,0.353480450914643,1.10664352764529));
#10331=CARTESIAN_POINT('Origin',(0.4739,0.349999999999997,1.1));
#10332=CARTESIAN_POINT('',(0.51,0.353480451097057,1.10664352740998));
#10333=CARTESIAN_POINT('',(0.46,0.353480451097057,1.10664352740998));
#10334=CARTESIAN_POINT('Origin',(0.51,0.350000000118451,1.09999999993794));
#10335=CARTESIAN_POINT('Origin',(0.46,0.350000000118451,1.09999999993794));
#10336=CARTESIAN_POINT('',(0.46,0.353480451097057,1.10664352740998));
#10337=CARTESIAN_POINT('Origin',(0.46,0.350000000118451,1.09999999993794));
#10338=CARTESIAN_POINT('',(0.461100000320458,0.353480451097057,1.10664352740998));
#10339=CARTESIAN_POINT('',(0.46,0.353480451097057,1.10664352740998));
#10340=CARTESIAN_POINT('Origin',(0.461100000229862,0.349999999881542,1.10000000006206));
#10341=CARTESIAN_POINT('Origin',(-0.459999999999996,0.349999999999997,1.1));
#10342=CARTESIAN_POINT('',(-0.459999999999996,0.35,1.115));
#10343=CARTESIAN_POINT('Origin',(-0.459999999999996,0.35,1.1));
#10344=CARTESIAN_POINT('Origin',(-0.488137499999996,0.349999999999997,1.1));
#10345=CARTESIAN_POINT('',(-0.488137499999996,0.353480450975115,1.10664352775337));
#10346=CARTESIAN_POINT('Origin',(-0.51,0.35,1.1));
#10347=CARTESIAN_POINT('',(0.46,0.35,1.115));
#10348=CARTESIAN_POINT('Origin',(0.46,0.35,1.1));
#10349=CARTESIAN_POINT('',(-0.51,0.35,1.115));
#10350=CARTESIAN_POINT('Origin',(-0.523137499999996,0.349999999999997,1.1));
#10351=CARTESIAN_POINT('',(-0.523137499999996,0.353480450975115,1.10664352775337));
#10352=CARTESIAN_POINT('Origin',(0.46,0.349999999999997,1.1));
#10353=CARTESIAN_POINT('Origin',(0.4468625,0.349999999999997,1.1));
#10354=CARTESIAN_POINT('',(0.4468625,0.353480450975115,1.10664352775337));
#10355=CARTESIAN_POINT('Origin',(-0.61,0.35,1.1));
#10356=CARTESIAN_POINT('Origin',(0.51,0.35,1.1));
#10357=CARTESIAN_POINT('',(1.04512838556094,2.20179512274211,1.82866726216848));
#10358=CARTESIAN_POINT('',(1.04512838556094,2.20179512274211,1.82866726216848));
#10359=CARTESIAN_POINT('',(1.04512838556094,2.20179512274211,1.82866726216848));
#10360=CARTESIAN_POINT('',(1.04512838556094,2.20179512274211,1.82866726216848));
#10361=CARTESIAN_POINT('',(1.04512838556094,2.20179512274211,1.82866726216848));
#10362=CARTESIAN_POINT('',(1.04512838556094,2.20179512274211,1.82866726216848));
#10363=CARTESIAN_POINT('',(1.04512838556094,2.20179512274211,1.82866726216848));
#10364=CARTESIAN_POINT('',(0.,0.,0.));
#10365=CARTESIAN_POINT('Origin',(-0.657,0.3,-0.955882353));
#10366=CARTESIAN_POINT('',(0.49,0.3,-0.945882353));
#10367=CARTESIAN_POINT('Origin',(0.49,0.3,-0.955882353));
#10368=CARTESIAN_POINT('',(0.5,0.3,-0.945882353));
#10369=CARTESIAN_POINT('',(-0.657,0.3,-0.945882353));
#10370=CARTESIAN_POINT('Origin',(0.5,0.3,-0.955882353));
#10371=CARTESIAN_POINT('Origin',(0.5,-6.21724893790088E-17,-1.74305014866149E-16));
#10372=CARTESIAN_POINT('',(0.499999999999679,-0.34999999999985,-0.999999999999358));
#10373=CARTESIAN_POINT('',(0.499999999999785,-0.34999999999985,0.999999999999358));
#10374=CARTESIAN_POINT('',(0.5,-0.35,-0.9999999995));
#10375=CARTESIAN_POINT('',(0.499999999999891,0.34999999999985,-0.999999999999358));
#10376=CARTESIAN_POINT('',(0.5,0.349999999825,-1.));
#10377=CARTESIAN_POINT('',(0.499999999999995,0.349999999999663,0.999999999999358));
#10378=CARTESIAN_POINT('',(0.5,0.35,0.9999999995));
#10379=CARTESIAN_POINT('',(0.5,-0.349999999825,1.));
#10380=CARTESIAN_POINT('',(0.5,-0.312833309,0.0299999999999509));
#10381=CARTESIAN_POINT('Origin',(0.5,-0.312833309,0.0249999999999754));
#10382=CARTESIAN_POINT('',(0.5,-0.270944436,-0.0200000000000491));
#10383=CARTESIAN_POINT('Origin',(0.5,-0.270944436,-0.0250000000000247));
#10384=CARTESIAN_POINT('',(0.5,0.3375,0.935));
#10385=CARTESIAN_POINT('Origin',(0.5,0.3375,0.94));
#10386=CARTESIAN_POINT('',(0.5,0.3375,0.975));
#10387=CARTESIAN_POINT('Origin',(0.5,0.3375,0.98));
#10388=CARTESIAN_POINT('',(0.5,0.3125,0.975));
#10389=CARTESIAN_POINT('Origin',(0.5,0.3125,0.98));
#10390=CARTESIAN_POINT('',(0.5,0.3125,0.935));
#10391=CARTESIAN_POINT('Origin',(0.5,0.3125,0.94));
#10392=CARTESIAN_POINT('',(0.5,-0.270944436,0.0299999999999509));
#10393=CARTESIAN_POINT('Origin',(0.5,-0.270944436,0.0249999999999754));
#10394=CARTESIAN_POINT('',(0.5,-0.312833309,-0.0200000000000491));
#10395=CARTESIAN_POINT('Origin',(0.5,-0.312833309,-0.0250000000000247));
#10396=CARTESIAN_POINT('Origin',(0.49,-6.21724893790088E-17,-1.74305014866149E-16));
#10397=CARTESIAN_POINT('',(0.490000000000164,-0.349999999999663,0.999999999999358));
#10398=CARTESIAN_POINT('',(0.490000000000005,0.349999999999663,0.999999999999358));
#10399=CARTESIAN_POINT('',(0.49,-0.349999999825,1.));
#10400=CARTESIAN_POINT('',(0.490000000000109,0.34999999999985,-0.999999999999358));
#10401=CARTESIAN_POINT('',(0.49,0.35,0.9999999995));
#10402=CARTESIAN_POINT('',(0.489999999999999,0.297099674089462,-1.00000000005445));
#10403=CARTESIAN_POINT('',(0.49,0.349999999825,-1.));
#10404=CARTESIAN_POINT('',(0.489999999999528,0.285766341000618,-0.990000000000234));
#10405=CARTESIAN_POINT('',(0.49,0.297099673879244,-0.999999999893451));
#10406=CARTESIAN_POINT('',(0.489999999999528,-0.339999999999815,-0.989999999999458));
#10407=CARTESIAN_POINT('',(0.49,0.285766340955704,-0.99));
#10408=CARTESIAN_POINT('',(0.48999999999979,-0.340000000000108,0.388147024999372));
#10409=CARTESIAN_POINT('',(0.49,-0.34,-0.9899999995));
#10410=CARTESIAN_POINT('',(0.489999999999525,-0.349999999999884,0.388147024999355));
#10411=CARTESIAN_POINT('',(0.49,-0.340000000375,0.388147024999997));
#10412=CARTESIAN_POINT('',(0.49,-0.35,0.38814702475));
#10413=CARTESIAN_POINT('',(0.49,-0.270944436,0.0299999999999512));
#10414=CARTESIAN_POINT('Origin',(0.49,-0.270944436,0.0249999999999756));
#10415=CARTESIAN_POINT('',(0.49,-0.270944436,-0.0200000000000489));
#10416=CARTESIAN_POINT('Origin',(0.49,-0.270944436,-0.0250000000000245));
#10417=CARTESIAN_POINT('',(0.49,0.3375,0.935));
#10418=CARTESIAN_POINT('Origin',(0.49,0.3375,0.94));
#10419=CARTESIAN_POINT('',(0.49,0.3375,0.975));
#10420=CARTESIAN_POINT('Origin',(0.49,0.3375,0.98));
#10421=CARTESIAN_POINT('',(0.49,0.3125,0.975));
#10422=CARTESIAN_POINT('Origin',(0.49,0.3125,0.98));
#10423=CARTESIAN_POINT('',(0.49,0.3125,0.935));
#10424=CARTESIAN_POINT('Origin',(0.49,0.3125,0.94));
#10425=CARTESIAN_POINT('',(0.49,-0.312833309,0.0299999999999512));
#10426=CARTESIAN_POINT('Origin',(0.49,-0.312833309,0.0249999999999756));
#10427=CARTESIAN_POINT('',(0.49,-0.312833309,-0.0200000000000489));
#10428=CARTESIAN_POINT('Origin',(0.49,-0.312833309,-0.0250000000000245));
#10429=CARTESIAN_POINT('Origin',(-0.61,-0.312833309,-0.025));
#10430=CARTESIAN_POINT('',(-0.61,-0.312833309,-0.0200000000000244));
#10431=CARTESIAN_POINT('Origin',(-0.61,-0.270944436,0.025));
#10432=CARTESIAN_POINT('',(-0.61,-0.270944436,0.0299999999999756));
#10433=CARTESIAN_POINT('Origin',(0.51,0.3125,0.94));
#10434=CARTESIAN_POINT('',(0.51,0.3125,0.935));
#10435=CARTESIAN_POINT('Origin',(0.51,0.3125,0.98));
#10436=CARTESIAN_POINT('',(0.51,0.3125,0.975));
#10437=CARTESIAN_POINT('Origin',(0.51,0.3375,0.98));
#10438=CARTESIAN_POINT('',(0.51,0.3375,0.975));
#10439=CARTESIAN_POINT('Origin',(0.51,0.3375,0.94));
#10440=CARTESIAN_POINT('',(0.51,0.3375,0.935));
#10441=CARTESIAN_POINT('Origin',(-0.61,-0.270944436,-0.025));
#10442=CARTESIAN_POINT('',(-0.61,-0.270944436,-0.0200000000000244));
#10443=CARTESIAN_POINT('Origin',(-0.61,-0.312833309,0.025));
#10444=CARTESIAN_POINT('',(-0.61,-0.312833309,0.0299999999999756));
#10445=CARTESIAN_POINT('Origin',(-8.71525074330748E-17,-6.21724893790088E-17,
-1.));
#10446=CARTESIAN_POINT('',(-0.499999999999892,0.349999999999775,-0.999999999999358));
#10447=CARTESIAN_POINT('',(-0.499999999999786,-0.349999999999775,-0.999999999999358));
#10448=CARTESIAN_POINT('',(-0.5,0.349999999825,-1.));
#10449=CARTESIAN_POINT('',(-0.490000000000108,0.349999999999775,-0.999999999999358));
#10450=CARTESIAN_POINT('',(-0.49000000025,0.35,-1.));
#10451=CARTESIAN_POINT('',(-0.489999999999988,0.297099674089289,-1.00000000005438));
#10452=CARTESIAN_POINT('',(-0.49,0.297099674375,-1.));
#10453=CARTESIAN_POINT('',(0.48999999975,0.297099674112451,-1.00000000009922));
#10454=CARTESIAN_POINT('',(0.49999999975,0.35,-1.));
#10455=CARTESIAN_POINT('',(-0.49999999975,-0.35,-1.));
#10456=CARTESIAN_POINT('Origin',(0.495,0.35,1.74305014866149E-16));
#10457=CARTESIAN_POINT('',(0.499999999997498,0.35,1.));
#10458=CARTESIAN_POINT('Origin',(0.495,-6.21724893790088E-17,1.));
#10459=CARTESIAN_POINT('',(0.499999999874375,-0.35,1.));
#10460=CARTESIAN_POINT('Origin',(-1.77635683940025E-17,-0.35,-1.74305014866149E-16));
#10461=CARTESIAN_POINT('',(-0.489999999999788,-0.349999999999849,0.388147024999355));
#10462=CARTESIAN_POINT('',(-0.48999999975,-0.35,0.388147024999997));
#10463=CARTESIAN_POINT('',(-0.490000000000164,-0.349999999999663,0.999999999999358));
#10464=CARTESIAN_POINT('',(-0.49,-0.35,0.9999999995));
#10465=CARTESIAN_POINT('',(-0.499999999999892,-0.349999999999775,0.999999999999358));
#10466=CARTESIAN_POINT('',(-0.49999999975,-0.35,1.));
#10467=CARTESIAN_POINT('',(-0.5,-0.35,-0.9999999995));
#10468=CARTESIAN_POINT('Origin',(6.68909372336657E-17,-0.345,0.388147024999997));
#10469=CARTESIAN_POINT('',(-0.489999999999907,-0.340000000000143,0.388147024999361));
#10470=CARTESIAN_POINT('',(-0.489999999755,-0.34,0.388147024999997));
#10471=CARTESIAN_POINT('',(-0.49,-0.349999999911875,0.388147024999998));
#10472=CARTESIAN_POINT('Origin',(-5.27355936696949E-17,-0.34,-0.3009264875));
#10473=CARTESIAN_POINT('',(-0.489999999999528,-0.339999999999815,-0.989999999999458));
#10474=CARTESIAN_POINT('',(0.489999999755,-0.34,-0.99));
#10475=CARTESIAN_POINT('',(-0.49,-0.34,-0.989999999655463));
#10476=CARTESIAN_POINT('Origin',(-6.68909372336657E-17,-0.0271168294999997,
-0.99));
#10477=CARTESIAN_POINT('',(-0.489999999999528,0.285766341000617,-0.990000000000234));
#10478=CARTESIAN_POINT('',(0.489999999755,0.285766341,-0.99));
#10479=CARTESIAN_POINT('',(-0.49,0.285766340843558,-0.99));
#10480=CARTESIAN_POINT('Origin',(-5.27355936696949E-17,0.2914330075,-0.995));
#10481=CARTESIAN_POINT('',(-0.49,0.297099673997167,-0.9999999999975));
#10482=CARTESIAN_POINT('Origin',(-0.495,0.35,1.74305014866149E-16));
#10483=CARTESIAN_POINT('',(-0.490000000000004,0.349999999999663,0.999999999999358));
#10484=CARTESIAN_POINT('',(-0.499999999999995,0.349999999999663,0.999999999999358));
#10485=CARTESIAN_POINT('',(-0.490000000002499,0.35,1.));
#10486=CARTESIAN_POINT('',(-0.489999999999999,0.35,-0.9999999995));
#10487=CARTESIAN_POINT('',(-0.499999999999999,0.35,0.9999999995));
#10488=CARTESIAN_POINT('Origin',(-0.49,-6.21724893790088E-17,-1.74305014866149E-16));
#10489=CARTESIAN_POINT('',(-0.49,-0.349999999825,1.));
#10490=CARTESIAN_POINT('',(-0.49,0.3,-0.945882353));
#10491=CARTESIAN_POINT('Origin',(-0.49,0.3,-0.955882353));
#10492=CARTESIAN_POINT('',(-0.49,-0.312833309,0.03));
#10493=CARTESIAN_POINT('Origin',(-0.49,-0.312833309,0.025));
#10494=CARTESIAN_POINT('',(-0.49,-0.270944436,-0.02));
#10495=CARTESIAN_POINT('Origin',(-0.49,-0.270944436,-0.025));
#10496=CARTESIAN_POINT('',(-0.49,0.3375,0.935));
#10497=CARTESIAN_POINT('Origin',(-0.49,0.3375,0.94));
#10498=CARTESIAN_POINT('',(-0.49,0.3375,0.975));
#10499=CARTESIAN_POINT('Origin',(-0.49,0.3375,0.98));
#10500=CARTESIAN_POINT('',(-0.49,0.3125,0.975));
#10501=CARTESIAN_POINT('Origin',(-0.49,0.3125,0.98));
#10502=CARTESIAN_POINT('',(-0.49,0.3125,0.935));
#10503=CARTESIAN_POINT('Origin',(-0.49,0.3125,0.94));
#10504=CARTESIAN_POINT('',(-0.49,-0.270944436,0.03));
#10505=CARTESIAN_POINT('Origin',(-0.49,-0.270944436,0.025));
#10506=CARTESIAN_POINT('',(-0.49,-0.312833309,-0.02));
#10507=CARTESIAN_POINT('Origin',(-0.49,-0.312833309,-0.025));
#10508=CARTESIAN_POINT('Origin',(-0.5,-6.21724893790088E-17,-1.74305014866149E-16));
#10509=CARTESIAN_POINT('',(-0.5,-0.349999999825,1.));
#10510=CARTESIAN_POINT('',(-0.5,0.3,-0.945882353));
#10511=CARTESIAN_POINT('Origin',(-0.5,0.3,-0.955882353));
#10512=CARTESIAN_POINT('',(-0.5,-0.270944436,0.03));
#10513=CARTESIAN_POINT('Origin',(-0.5,-0.270944436,0.025));
#10514=CARTESIAN_POINT('',(-0.5,-0.270944436,-0.02));
#10515=CARTESIAN_POINT('Origin',(-0.5,-0.270944436,-0.025));
#10516=CARTESIAN_POINT('',(-0.5,0.3375,0.935));
#10517=CARTESIAN_POINT('Origin',(-0.5,0.3375,0.94));
#10518=CARTESIAN_POINT('',(-0.5,0.3375,0.975));
#10519=CARTESIAN_POINT('Origin',(-0.5,0.3375,0.98));
#10520=CARTESIAN_POINT('',(-0.5,0.3125,0.975));
#10521=CARTESIAN_POINT('Origin',(-0.5,0.3125,0.98));
#10522=CARTESIAN_POINT('',(-0.5,0.3125,0.935));
#10523=CARTESIAN_POINT('Origin',(-0.5,0.3125,0.94));
#10524=CARTESIAN_POINT('',(-0.5,-0.312833309,0.03));
#10525=CARTESIAN_POINT('Origin',(-0.5,-0.312833309,0.025));
#10526=CARTESIAN_POINT('',(-0.5,-0.312833309,-0.02));
#10527=CARTESIAN_POINT('Origin',(-0.5,-0.312833309,-0.025));
#10528=CARTESIAN_POINT('Origin',(-0.495,-6.21724893790088E-17,1.));
#10529=CARTESIAN_POINT('Origin',(-0.61,-0.312833309,-0.025));
#10530=CARTESIAN_POINT('',(-0.61,-0.312833309,-0.02));
#10531=CARTESIAN_POINT('Origin',(-0.61,-0.270944436,0.025));
#10532=CARTESIAN_POINT('',(-0.61,-0.270944436,0.03));
#10533=CARTESIAN_POINT('Origin',(0.51,0.3125,0.94));
#10534=CARTESIAN_POINT('',(0.51,0.3125,0.935));
#10535=CARTESIAN_POINT('Origin',(0.51,0.3125,0.98));
#10536=CARTESIAN_POINT('',(0.51,0.3125,0.975));
#10537=CARTESIAN_POINT('Origin',(0.51,0.3375,0.98));
#10538=CARTESIAN_POINT('',(0.51,0.3375,0.975));
#10539=CARTESIAN_POINT('Origin',(0.51,0.3375,0.94));
#10540=CARTESIAN_POINT('',(0.51,0.3375,0.935));
#10541=CARTESIAN_POINT('Origin',(-0.61,-0.270944436,-0.025));
#10542=CARTESIAN_POINT('',(-0.61,-0.270944436,-0.02));
#10543=CARTESIAN_POINT('Origin',(-0.61,-0.312833309,0.025));
#10544=CARTESIAN_POINT('',(-0.61,-0.312833309,0.03));
#10545=CARTESIAN_POINT('Origin',(-0.657,0.3,-0.955882353));
#10546=CARTESIAN_POINT('',(-0.657,0.3,-0.945882353));
#10547=CARTESIAN_POINT('',(0.,0.,0.));
#10548=CARTESIAN_POINT('Origin',(0.5,-0.549047301,0.966510346));
#10549=CARTESIAN_POINT('',(0.475,-0.549047301,0.963510346));
#10550=CARTESIAN_POINT('Origin',(0.475,-0.549047301,0.966510346));
#10551=CARTESIAN_POINT('',(0.5,-0.549047301,0.963510346));
#10552=CARTESIAN_POINT('',(0.5,-0.549047301,0.963510346));
#10553=CARTESIAN_POINT('Origin',(0.5,-0.549047301,0.966510346));
#10554=CARTESIAN_POINT('Origin',(0.5,-0.549047301000001,0.966510346));
#10555=CARTESIAN_POINT('Origin',(0.475,-0.549047301,0.966510346));
#10556=CARTESIAN_POINT('',(0.475,-0.549047301,0.954010346));
#10557=CARTESIAN_POINT('Origin',(0.475,-0.549047301,0.966510346));
#10558=CARTESIAN_POINT('Origin',(0.475,-0.549047301,0.966510346));
#10559=CARTESIAN_POINT('',(-0.475,-0.549047301,0.954010346));
#10560=CARTESIAN_POINT('Origin',(-0.475,-0.549047301,0.966510346));
#10561=CARTESIAN_POINT('',(0.475,-0.549047301,0.954010346));
#10562=CARTESIAN_POINT('Origin',(-0.475,-0.549047301,0.966510346));
#10563=CARTESIAN_POINT('',(-0.475,-0.549047301,0.963510346));
#10564=CARTESIAN_POINT('Origin',(-0.475,-0.549047301,0.966510346));
#10565=CARTESIAN_POINT('Origin',(0.5,-0.549047301,0.966510346));
#10566=CARTESIAN_POINT('',(-0.5,-0.549047301,0.963510346));
#10567=CARTESIAN_POINT('Origin',(-0.5,-0.549047301,0.966510346));
#10568=CARTESIAN_POINT('',(0.5,-0.549047301,0.963510346));
#10569=CARTESIAN_POINT('Origin',(-0.5,-0.549047301000001,0.966510346));
#10570=CARTESIAN_POINT('',(0.,0.,0.));
#10571=CARTESIAN_POINT('',(0.,0.,0.));
#10572=CARTESIAN_POINT('Origin',(0.493,-0.542782557,0.975695518));
#10573=CARTESIAN_POINT('',(0.493,-0.542782557,0.974505818));
#10574=CARTESIAN_POINT('Origin',(0.493,-0.542782557,0.975695518));
#10575=CARTESIAN_POINT('',(0.49,-0.542782557,0.974505818));
#10576=CARTESIAN_POINT('',(0.493,-0.542782557,0.974505818));
#10577=CARTESIAN_POINT('Origin',(0.49,-0.542782557,0.975695518));
#10578=CARTESIAN_POINT('Origin',(0.493,-0.545454380845135,0.969136388159038));
#10579=CARTESIAN_POINT('',(0.493,-0.534613544999688,0.966510345999423));
#10580=CARTESIAN_POINT('',(0.493,-0.541830423000466,0.979010345999528));
#10581=CARTESIAN_POINT('',(0.493,-0.534613544872232,0.9665103457787));
#10582=CARTESIAN_POINT('',(0.492999999985368,-0.552655740191489,0.972760346019922));
#10583=CARTESIAN_POINT('',(0.493,-0.541830423323753,0.979010345813081));
#10584=CARTESIAN_POINT('',(0.493,-0.545438862110786,0.960260346041367));
#10585=CARTESIAN_POINT('Origin',(0.493,-0.549047301,0.966510346));
#10586=CARTESIAN_POINT('',(0.493,-0.545438862219975,0.960260345872998));
#10587=CARTESIAN_POINT('',(0.493,-0.537960337,0.966153487));
#10588=CARTESIAN_POINT('Origin',(0.493,-0.537960337,0.967343188));
#10589=CARTESIAN_POINT('Origin',(0.493,-0.537960337,0.967343188));
#10590=CARTESIAN_POINT('',(0.49,-0.537960337,0.966153487));
#10591=CARTESIAN_POINT('',(0.493,-0.537960337,0.966153487));
#10592=CARTESIAN_POINT('Origin',(0.49,-0.537960337,0.967343188));
#10593=CARTESIAN_POINT('Origin',(0.4915,-0.5400262035,0.963385346000001));
#10594=CARTESIAN_POINT('',(0.490000000000001,-0.545438861975815,0.960260346119293));
#10595=CARTESIAN_POINT('',(0.490000000000002,-0.545438862,0.960260346000001));
#10596=CARTESIAN_POINT('',(0.490000000000001,-0.53461354500041,0.966510345999764));
#10597=CARTESIAN_POINT('',(0.490000000000002,-0.534613545008309,0.966510345995204));
#10598=CARTESIAN_POINT('',(0.493000000000002,-0.534613545,0.966510346000001));
#10599=CARTESIAN_POINT('Origin',(0.493,-0.549047301,0.966510346));
#10600=CARTESIAN_POINT('',(0.490000000000001,-0.552655740263515,0.972760345829652));
#10601=CARTESIAN_POINT('',(0.49000000025,-0.552655739997383,0.972760345685524));
#10602=CARTESIAN_POINT('Origin',(0.49,-0.549047301,0.966510346));
#10603=CARTESIAN_POINT('Origin',(0.4915,-0.547243082,0.975885346));
#10604=CARTESIAN_POINT('',(0.49,-0.541830423,0.979010346));
#10605=CARTESIAN_POINT('',(0.490000000000002,-0.541830423,0.979010346));
#10606=CARTESIAN_POINT('',(0.490000000000002,-0.552655740692886,0.972760346177312));
#10607=CARTESIAN_POINT('Origin',(0.4915,-0.538221983999999,0.972760345999999));
#10608=CARTESIAN_POINT('',(0.490000000000002,-0.541830422999999,0.979010346));
#10609=CARTESIAN_POINT('Origin',(0.49,-0.545454380845135,0.969136388159038));
#10610=CARTESIAN_POINT('',(0.,0.,0.));
#10611=CARTESIAN_POINT('Origin',(-5.27355936696949E-17,-0.275347663,0.388147024999997));
#10612=CARTESIAN_POINT('',(-0.489999999999528,-0.349999999999892,0.38814702499999));
#10613=CARTESIAN_POINT('',(-0.489999999999528,-0.200695326000145,0.388147024999907));
#10614=CARTESIAN_POINT('',(-0.49,-0.349999999962674,0.388147024999997));
#10615=CARTESIAN_POINT('',(0.489999999999528,-0.349999999999892,0.38814702499999));
#10616=CARTESIAN_POINT('',(0.489999999755,-0.35,0.388147024999997));
#10617=CARTESIAN_POINT('',(0.489999999999528,-0.200695326000145,0.388147024999907));
#10618=CARTESIAN_POINT('',(0.49,-0.200695326040595,0.388147024999997));
#10619=CARTESIAN_POINT('',(-0.489999999755,-0.200695326,0.388147024999997));
#10620=CARTESIAN_POINT('Origin',(-5.27355936696949E-17,-0.35,0.383147025));
#10621=CARTESIAN_POINT('',(-0.489999999999528,-0.349999999999892,0.378147025000008));
#10622=CARTESIAN_POINT('',(-0.49,-0.35,0.3781470250025));
#10623=CARTESIAN_POINT('',(0.489999999999528,-0.349999999999892,0.378147025000008));
#10624=CARTESIAN_POINT('',(0.489999999755,-0.35,0.378147025));
#10625=CARTESIAN_POINT('',(0.49,-0.35,0.3881470249975));
#10626=CARTESIAN_POINT('Origin',(0.49,-0.275347663043444,0.383147025));
#10627=CARTESIAN_POINT('',(0.489999999999528,-0.201776321000629,0.378147024999632));
#10628=CARTESIAN_POINT('',(0.49,-0.201776321653339,0.378147025));
#10629=CARTESIAN_POINT('',(0.49,-0.200695326001004,0.388147024990716));
#10630=CARTESIAN_POINT('Origin',(-0.49,-0.275347663043444,0.383147025));
#10631=CARTESIAN_POINT('',(-0.489999999999528,-0.201776321000629,0.378147024999632));
#10632=CARTESIAN_POINT('',(-0.49,-0.200695326001004,0.388147024990716));
#10633=CARTESIAN_POINT('',(-0.49,-0.201776321653339,0.378147025));
#10634=CARTESIAN_POINT('Origin',(-6.68909372336657E-17,-0.2758881605,0.378147025000002));
#10635=CARTESIAN_POINT('',(0.489999999755,-0.201776321,0.378147025000002));
#10636=CARTESIAN_POINT('Origin',(-5.27355936696949E-17,-0.2012358235,0.383147025));
#10637=CARTESIAN_POINT('',(0.,0.,0.));
#10638=CARTESIAN_POINT('Origin',(-0.493,-0.542782557,0.975695518));
#10639=CARTESIAN_POINT('',(-0.493,-0.542782557,0.976885218));
#10640=CARTESIAN_POINT('Origin',(-0.493,-0.542782557,0.975695518));
#10641=CARTESIAN_POINT('',(-0.49,-0.542782557,0.976885218));
#10642=CARTESIAN_POINT('',(-0.493,-0.542782557,0.976885218));
#10643=CARTESIAN_POINT('Origin',(-0.49,-0.542782557,0.975695518));
#10644=CARTESIAN_POINT('Origin',(-0.493,-0.545454380845136,0.969136388159038));
#10645=CARTESIAN_POINT('',(-0.493,-0.541830423000466,0.979010345999528));
#10646=CARTESIAN_POINT('',(-0.493,-0.534613544999688,0.966510345999423));
#10647=CARTESIAN_POINT('',(-0.493,-0.541830422948787,0.979010345911298));
#10648=CARTESIAN_POINT('',(-0.492999999983539,-0.545438861934028,0.9602603461963));
#10649=CARTESIAN_POINT('',(-0.493,-0.534613545009254,0.966510345994658));
#10650=CARTESIAN_POINT('',(-0.493,-0.552655740808602,0.972760345664227));
#10651=CARTESIAN_POINT('Origin',(-0.493,-0.549047301,0.966510346));
#10652=CARTESIAN_POINT('',(-0.493,-0.552655741001846,0.972760345998934));
#10653=CARTESIAN_POINT('',(-0.493,-0.537960337,0.968532889));
#10654=CARTESIAN_POINT('Origin',(-0.493,-0.537960337,0.967343188));
#10655=CARTESIAN_POINT('Origin',(-0.493,-0.537960337,0.967343188));
#10656=CARTESIAN_POINT('',(-0.49,-0.537960337,0.968532889));
#10657=CARTESIAN_POINT('',(-0.493,-0.537960337,0.968532889));
#10658=CARTESIAN_POINT('Origin',(-0.49,-0.537960337,0.967343188));
#10659=CARTESIAN_POINT('Origin',(-0.4915,-0.547243082,0.975885346));
#10660=CARTESIAN_POINT('',(-0.49,-0.552655740613422,0.972760345925411));
#10661=CARTESIAN_POINT('',(-0.49,-0.552655741,0.972760346));
#10662=CARTESIAN_POINT('',(-0.49,-0.541830423,0.979010346));
#10663=CARTESIAN_POINT('',(-0.49,-0.541830423,0.979010346));
#10664=CARTESIAN_POINT('',(-0.493,-0.541830423,0.979010346));
#10665=CARTESIAN_POINT('Origin',(-0.493,-0.549047301,0.966510346));
#10666=CARTESIAN_POINT('',(-0.49,-0.54543886200176,0.960260346156978));
#10667=CARTESIAN_POINT('',(-0.49000000025,-0.545438862001176,0.960260346315308));
#10668=CARTESIAN_POINT('Origin',(-0.49,-0.549047301,0.966510346));
#10669=CARTESIAN_POINT('Origin',(-0.4915,-0.5400262035,0.963385346000001));
#10670=CARTESIAN_POINT('',(-0.49,-0.534613545,0.966510346));
#10671=CARTESIAN_POINT('',(-0.49,-0.534613545,0.966510346000001));
#10672=CARTESIAN_POINT('',(-0.49,-0.545438861933347,0.960260346038483));
#10673=CARTESIAN_POINT('Origin',(-0.4915,-0.538221983999999,0.972760345999999));
#10674=CARTESIAN_POINT('',(-0.49,-0.534613544999999,0.966510346));
#10675=CARTESIAN_POINT('Origin',(-0.49,-0.545454380845136,0.969136388159038));
#10676=CARTESIAN_POINT('',(0.,0.,0.));
#10677=CARTESIAN_POINT('Origin',(-0.61,-0.537960337,0.967343188));
#10678=CARTESIAN_POINT('',(-0.49,-0.537960337,0.968532889));
#10679=CARTESIAN_POINT('Origin',(-0.49,-0.537960337,0.967343188));
#10680=CARTESIAN_POINT('',(-0.48,-0.537960337,0.968532889));
#10681=CARTESIAN_POINT('',(-0.61,-0.537960337,0.968532889));
#10682=CARTESIAN_POINT('Origin',(-0.48,-0.537960337,0.967343188));
#10683=CARTESIAN_POINT('Origin',(0.49,-0.3734279375,0.289236489));
#10684=CARTESIAN_POINT('',(0.489999999999839,-0.546160549999463,0.97651034600006));
#10685=CARTESIAN_POINT('',(0.489999999999929,-0.541830422999722,0.979010345999397));
#10686=CARTESIAN_POINT('',(0.49,-0.546160549333911,0.976510346384566));
#10687=CARTESIAN_POINT('',(0.49,-0.205841846999809,0.387061060999092));
#10688=CARTESIAN_POINT('',(0.49,-0.205841846899785,0.387061060826422));
#10689=CARTESIAN_POINT('',(0.489999999999528,-0.290922804999604,-0.400000000000061));
#10690=CARTESIAN_POINT('',(0.49,-0.290922805000769,-0.400000000007112));
#10691=CARTESIAN_POINT('',(0.489999999999528,-0.285951764999811,-0.400537366999761));
#10692=CARTESIAN_POINT('',(0.49,-0.28595176493698,-0.400537367006812));
#10693=CARTESIAN_POINT('',(0.49,-0.200695325999748,0.388147024998802));
#10694=CARTESIAN_POINT('',(0.49,-0.20069532607737,0.388147024284284));
#10695=CARTESIAN_POINT('',(0.49,-0.541830422462856,0.979010345069641));
#10696=CARTESIAN_POINT('',(0.49,-0.542782557,0.976885219000204));
#10697=CARTESIAN_POINT('Origin',(0.49,-0.542782557,0.975695518000103));
#10698=CARTESIAN_POINT('',(0.49,-0.537960337,0.968532889000204));
#10699=CARTESIAN_POINT('Origin',(0.49,-0.537960337,0.967343188000103));
#10700=CARTESIAN_POINT('Origin',(-5.27355936696949E-17,-0.3760011985,0.6817857035));
#10701=CARTESIAN_POINT('',(-0.479999999999998,-0.537552110829253,0.961600091996557));
#10702=CARTESIAN_POINT('',(0.479999999999998,-0.537552110829253,0.961600091996557));
#10703=CARTESIAN_POINT('',(-0.479999999395,-0.537552110814951,0.961600092000007));
#10704=CARTESIAN_POINT('',(-0.479999999999894,-0.546160550000244,0.976510345999441));
#10705=CARTESIAN_POINT('',(-0.48,-0.54616054991492,0.976510345852638));
#10706=CARTESIAN_POINT('',(-0.489999999999894,-0.546160549999321,0.976510346000143));
#10707=CARTESIAN_POINT('',(-0.489999999755,-0.54616055,0.976510346));
#10708=CARTESIAN_POINT('',(-0.49,-0.205841846999808,0.387061060999092));
#10709=CARTESIAN_POINT('',(-0.49,-0.20584184708508,0.387061061147362));
#10710=CARTESIAN_POINT('',(0.489999999755,-0.205841847,0.387061061));
#10711=CARTESIAN_POINT('',(0.479999999999928,-0.546160550000382,0.976510345999348));
#10712=CARTESIAN_POINT('',(0.479999999971875,-0.54616055,0.976510346));
#10713=CARTESIAN_POINT('',(0.48,-0.537552110906866,0.961600092100691));
#10714=CARTESIAN_POINT('Origin',(-5.27355936696949E-17,-0.248382326,-0.00646946950000008));
#10715=CARTESIAN_POINT('',(-0.48999999999979,-0.290922804999483,-0.400000000000166));
#10716=CARTESIAN_POINT('',(-0.49,-0.29092280497873,-0.399999999803235));
#10717=CARTESIAN_POINT('',(0.489999999755,-0.290922805,-0.4));
#10718=CARTESIAN_POINT('Origin',(-5.27355936696949E-17,-0.288437285,-0.4002686835));
#10719=CARTESIAN_POINT('',(-0.489999999999528,-0.285951764999492,-0.400537366999852));
#10720=CARTESIAN_POINT('',(-0.49,-0.285951765001243,-0.400537366999866));
#10721=CARTESIAN_POINT('',(0.489999999755,-0.285951765,-0.400537367));
#10722=CARTESIAN_POINT('Origin',(-5.27355936696949E-17,-0.243323545500001,
-0.00619517099999993));
#10723=CARTESIAN_POINT('',(-0.49,-0.200695325999748,0.388147024998802));
#10724=CARTESIAN_POINT('',(-0.49,-0.200695326026299,0.388147024756719));
#10725=CARTESIAN_POINT('',(0.489999999755,-0.200695326000001,0.388147025));
#10726=CARTESIAN_POINT('Origin',(-5.27355936696949E-17,-0.3712628745,0.6835786855));
#10727=CARTESIAN_POINT('',(-0.479999999999952,-0.541830423000291,0.979010345999481));
#10728=CARTESIAN_POINT('',(-0.489999999999929,-0.541830422999722,0.979010345999397));
#10729=CARTESIAN_POINT('',(-0.479999999971875,-0.541830423,0.979010346000001));
#10730=CARTESIAN_POINT('',(-0.479999999999922,-0.531778608197404,0.961600092003128));
#10731=CARTESIAN_POINT('',(-0.48,-0.531778608296587,0.961600092203291));
#10732=CARTESIAN_POINT('',(0.479999999999995,-0.531778608197352,0.961600092003097));
#10733=CARTESIAN_POINT('',(0.479999999395,-0.531778608211303,0.961600092000007));
#10734=CARTESIAN_POINT('',(0.479999999999952,-0.541830423000291,0.979010345999482));
#10735=CARTESIAN_POINT('',(0.48,-0.541830422911468,0.979010345846659));
#10736=CARTESIAN_POINT('',(0.489999999755,-0.541830423,0.979010346000001));
#10737=CARTESIAN_POINT('',(-0.49,-0.541830422710406,0.979010345498409));
#10738=CARTESIAN_POINT('Origin',(-0.48,-0.5389695795,0.970305218737048));
#10739=CARTESIAN_POINT('',(-0.48,-0.541830423513964,0.979010345703262));
#10740=CARTESIAN_POINT('',(-0.48,-0.537552111040899,0.961600092));
#10741=CARTESIAN_POINT('',(-0.48,-0.542782557,0.976885219));
#10742=CARTESIAN_POINT('Origin',(-0.48,-0.542782557,0.975695518));
#10743=CARTESIAN_POINT('Origin',(-0.485,-0.543995486499999,0.977760346));
#10744=CARTESIAN_POINT('',(-0.49,-0.546160549666815,0.976510346192364));
#10745=CARTESIAN_POINT('Origin',(-0.49,-0.3734279375,0.289236489));
#10746=CARTESIAN_POINT('',(-0.49,-0.542782557,0.976885219));
#10747=CARTESIAN_POINT('Origin',(-0.49,-0.542782557,0.975695518));
#10748=CARTESIAN_POINT('Origin',(0.485,-0.543995486499999,0.977760346));
#10749=CARTESIAN_POINT('',(0.48,-0.54616055,0.976510346));
#10750=CARTESIAN_POINT('Origin',(0.48,-0.5389695795,0.970305218737048));
#10751=CARTESIAN_POINT('',(0.48,-0.537552111040899,0.961600092));
#10752=CARTESIAN_POINT('',(0.48,-0.542782557,0.976885219000204));
#10753=CARTESIAN_POINT('Origin',(0.48,-0.542782557,0.975695518000102));
#10754=CARTESIAN_POINT('',(0.48,-0.537960337,0.968532889000204));
#10755=CARTESIAN_POINT('Origin',(0.48,-0.537960337,0.967343188000102));
#10756=CARTESIAN_POINT('Origin',(8.79851747015437E-17,-0.5346653595,0.961600092000007));
#10757=CARTESIAN_POINT('Origin',(-0.61,-0.537960337,0.967343188));
#10758=CARTESIAN_POINT('',(-0.61,-0.537960337,0.968532889000102));
#10759=CARTESIAN_POINT('Origin',(-0.61,-0.542782557,0.975695518));
#10760=CARTESIAN_POINT('',(-0.61,-0.542782557,0.976885219000102));
#10761=CARTESIAN_POINT('Origin',(-0.61,-0.542782557,0.975695518));
#10762=CARTESIAN_POINT('',(-0.61,-0.542782557,0.976885219));
#10763=CARTESIAN_POINT('',(0.,0.,0.));
#10764=CARTESIAN_POINT('Origin',(0.477,-0.542782557,0.975695518));
#10765=CARTESIAN_POINT('',(0.477,-0.542782557,0.976885218));
#10766=CARTESIAN_POINT('Origin',(0.477,-0.542782557,0.975695518));
#10767=CARTESIAN_POINT('',(0.48,-0.542782557,0.976885218));
#10768=CARTESIAN_POINT('',(0.477,-0.542782557,0.976885218));
#10769=CARTESIAN_POINT('Origin',(0.48,-0.542782557,0.975695518));
#10770=CARTESIAN_POINT('Origin',(0.477,-0.545454380845136,0.969136388159038));
#10771=CARTESIAN_POINT('',(0.477,-0.541830423000466,0.979010345999528));
#10772=CARTESIAN_POINT('',(0.477,-0.534613544999688,0.966510345999423));
#10773=CARTESIAN_POINT('',(0.477,-0.541830422948787,0.979010345911298));
#10774=CARTESIAN_POINT('',(0.477000000016461,-0.545438861934028,0.9602603461963));
#10775=CARTESIAN_POINT('',(0.477,-0.534613545009254,0.966510345994658));
#10776=CARTESIAN_POINT('',(0.477,-0.552655740808602,0.972760345664227));
#10777=CARTESIAN_POINT('Origin',(0.477,-0.549047301,0.966510346));
#10778=CARTESIAN_POINT('',(0.477,-0.552655741001846,0.972760345998934));
#10779=CARTESIAN_POINT('',(0.477,-0.537960337,0.968532889));
#10780=CARTESIAN_POINT('Origin',(0.477,-0.537960337,0.967343188));
#10781=CARTESIAN_POINT('Origin',(0.477,-0.537960337,0.967343188));
#10782=CARTESIAN_POINT('',(0.48,-0.537960337,0.968532889));
#10783=CARTESIAN_POINT('',(0.477,-0.537960337,0.968532889));
#10784=CARTESIAN_POINT('Origin',(0.48,-0.537960337,0.967343188));
#10785=CARTESIAN_POINT('Origin',(0.4785,-0.547243082,0.975885346));
#10786=CARTESIAN_POINT('',(0.48,-0.552655740613422,0.972760345925411));
#10787=CARTESIAN_POINT('',(0.479999999999999,-0.552655741,0.972760346));
#10788=CARTESIAN_POINT('',(0.48,-0.541830423,0.979010346));
#10789=CARTESIAN_POINT('',(0.479999999999999,-0.541830423,0.979010346));
#10790=CARTESIAN_POINT('',(0.476999999999999,-0.541830423,0.979010346));
#10791=CARTESIAN_POINT('Origin',(0.477,-0.549047301,0.966510346));
#10792=CARTESIAN_POINT('',(0.48,-0.54543886200176,0.960260346156978));
#10793=CARTESIAN_POINT('',(0.47999999975,-0.545438862001176,0.960260346315308));
#10794=CARTESIAN_POINT('Origin',(0.48,-0.549047301,0.966510346));
#10795=CARTESIAN_POINT('Origin',(0.4785,-0.5400262035,0.963385346000001));
#10796=CARTESIAN_POINT('',(0.48,-0.534613545,0.966510346));
#10797=CARTESIAN_POINT('',(0.479999999999999,-0.534613545,0.966510346000001));
#10798=CARTESIAN_POINT('',(0.479999999999999,-0.545438861933347,0.960260346038483));
#10799=CARTESIAN_POINT('Origin',(0.4785,-0.538221983999999,0.972760345999999));
#10800=CARTESIAN_POINT('',(0.479999999999999,-0.534613544999999,0.966510346));
#10801=CARTESIAN_POINT('Origin',(0.48,-0.545454380845136,0.969136388159038));
#10802=CARTESIAN_POINT('',(0.,0.,0.));
#10803=CARTESIAN_POINT('Origin',(-0.477,-0.542782557,0.975695518));
#10804=CARTESIAN_POINT('',(-0.477,-0.542782557,0.974505818));
#10805=CARTESIAN_POINT('Origin',(-0.477,-0.542782557,0.975695518));
#10806=CARTESIAN_POINT('',(-0.48,-0.542782557,0.974505818));
#10807=CARTESIAN_POINT('',(-0.477,-0.542782557,0.974505818));
#10808=CARTESIAN_POINT('Origin',(-0.48,-0.542782557,0.975695518));
#10809=CARTESIAN_POINT('Origin',(-0.477,-0.545454380845135,0.969136388159038));
#10810=CARTESIAN_POINT('',(-0.477,-0.534613544999688,0.966510345999423));
#10811=CARTESIAN_POINT('',(-0.477,-0.541830423000466,0.979010345999528));
#10812=CARTESIAN_POINT('',(-0.477,-0.534613544872232,0.9665103457787));
#10813=CARTESIAN_POINT('',(-0.477000000014632,-0.552655740191489,0.972760346019922));
#10814=CARTESIAN_POINT('',(-0.477,-0.541830423323753,0.979010345813081));
#10815=CARTESIAN_POINT('',(-0.477,-0.545438862110786,0.960260346041367));
#10816=CARTESIAN_POINT('Origin',(-0.477,-0.549047301,0.966510346));
#10817=CARTESIAN_POINT('',(-0.477,-0.545438862219975,0.960260345872998));
#10818=CARTESIAN_POINT('',(-0.477,-0.537960337,0.966153487));
#10819=CARTESIAN_POINT('Origin',(-0.477,-0.537960337,0.967343188));
#10820=CARTESIAN_POINT('Origin',(-0.477,-0.537960337,0.967343188));
#10821=CARTESIAN_POINT('',(-0.48,-0.537960337,0.966153487));
#10822=CARTESIAN_POINT('',(-0.477,-0.537960337,0.966153487));
#10823=CARTESIAN_POINT('Origin',(-0.48,-0.537960337,0.967343188));
#10824=CARTESIAN_POINT('Origin',(-0.4785,-0.5400262035,0.963385346000001));
#10825=CARTESIAN_POINT('',(-0.48,-0.545438861975815,0.960260346119293));
#10826=CARTESIAN_POINT('',(-0.479999999999999,-0.545438862,0.960260346000001));
#10827=CARTESIAN_POINT('',(-0.479999999999999,-0.53461354500041,0.966510345999764));
#10828=CARTESIAN_POINT('',(-0.479999999999999,-0.534613545008309,0.966510345995204));
#10829=CARTESIAN_POINT('',(-0.476999999999999,-0.534613545,0.966510346000001));
#10830=CARTESIAN_POINT('Origin',(-0.477,-0.549047301,0.966510346));
#10831=CARTESIAN_POINT('',(-0.48,-0.552655740263515,0.972760345829652));
#10832=CARTESIAN_POINT('',(-0.47999999975,-0.552655739997383,0.972760345685524));
#10833=CARTESIAN_POINT('Origin',(-0.48,-0.549047301,0.966510346));
#10834=CARTESIAN_POINT('Origin',(-0.4785,-0.547243082,0.975885346));
#10835=CARTESIAN_POINT('',(-0.48,-0.541830423,0.979010346));
#10836=CARTESIAN_POINT('',(-0.479999999999999,-0.541830423,0.979010346));
#10837=CARTESIAN_POINT('',(-0.479999999999999,-0.552655740692886,0.972760346177312));
#10838=CARTESIAN_POINT('Origin',(-0.4785,-0.538221983999999,0.972760345999999));
#10839=CARTESIAN_POINT('',(-0.479999999999999,-0.541830422999999,0.979010346));
#10840=CARTESIAN_POINT('Origin',(-0.48,-0.545454380845135,0.969136388159038));
#10841=CARTESIAN_POINT('',(1.04512838556094,1.66136027488207,1.86547237816828));
#10842=CARTESIAN_POINT('',(1.04512838556094,1.66136027488207,1.86547237816828));
#10843=CARTESIAN_POINT('',(1.04512838556094,1.66136027488207,1.86547237816828));
#10844=CARTESIAN_POINT('',(1.04512838556094,1.66136027488207,1.86547237816828));
#10845=CARTESIAN_POINT('',(1.04512838556094,1.66136027488207,1.86547237816828));
#10846=CARTESIAN_POINT('',(1.04512838556094,1.66136027488207,1.86547237816828));
#10847=CARTESIAN_POINT('',(0.,0.,0.));
#10848=CARTESIAN_POINT('',(0.,0.,0.));
#10849=CARTESIAN_POINT('Origin',(-0.560710678,0.3,-0.955882353));
#10850=CARTESIAN_POINT('',(0.3,0.283459459165354,-0.974628299273763));
#10851=CARTESIAN_POINT('',(0.29999999999996,0.316540540959,-0.937136406587632));
#10852=CARTESIAN_POINT('Origin',(0.3,0.300000000061598,-0.955882352930187));
#10853=CARTESIAN_POINT('Origin',(0.3,0.300000000061598,-0.955882352930187));
#10854=CARTESIAN_POINT('Origin',(0.3,0.716460202,-1.323347237));
#10855=CARTESIAN_POINT('',(0.29999999999999,0.706540540912883,-1.28125405363754));
#10856=CARTESIAN_POINT('',(0.3,0.733000742863165,-1.30460129069508));
#10857=CARTESIAN_POINT('',(0.299999999999999,0.673459459119104,-1.31874594632356));
#10858=CARTESIAN_POINT('Origin',(0.3,0.690000000016651,-1.29999999998113));
#10859=CARTESIAN_POINT('Origin',(0.3,0.690000000016651,-1.29999999998113));
#10860=CARTESIAN_POINT('Origin',(0.35,0.69,-1.3));
#10861=CARTESIAN_POINT('',(0.,0.,0.));
#10862=CARTESIAN_POINT('Origin',(-0.560710678,0.3,-0.955882353));
#10863=CARTESIAN_POINT('',(0.49,0.3,-0.930882353));
#10864=CARTESIAN_POINT('Origin',(0.49,0.3,-0.955882353));
#10865=CARTESIAN_POINT('',(-0.49,0.3,-0.930882353));
#10866=CARTESIAN_POINT('',(-0.560710678,0.3,-0.930882353));
#10867=CARTESIAN_POINT('Origin',(-0.49,0.3,-0.955882353));
#10868=CARTESIAN_POINT('Origin',(-0.49,0.3,-0.955882352999999));
#10869=CARTESIAN_POINT('Origin',(0.49,0.3,-0.955882352999999));
#10870=CARTESIAN_POINT('',(0.,0.,0.));
#10871=CARTESIAN_POINT('Origin',(0.27,0.69,-1.3));
#10872=CARTESIAN_POINT('',(0.27,0.69,-1.325));
#10873=CARTESIAN_POINT('Origin',(0.27,0.69,-1.3));
#10874=CARTESIAN_POINT('',(-0.27,0.69,-1.325));
#10875=CARTESIAN_POINT('',(0.27,0.69,-1.325));
#10876=CARTESIAN_POINT('Origin',(-0.27,0.69,-1.3));
#10877=CARTESIAN_POINT('Origin',(-0.27,0.69,-1.3));
#10878=CARTESIAN_POINT('',(-0.27,0.69,-1.335));
#10879=CARTESIAN_POINT('Origin',(-0.27,0.69,-1.3));
#10880=CARTESIAN_POINT('Origin',(0.27,0.69,-1.3));
#10881=CARTESIAN_POINT('',(0.27,0.69,-1.335));
#10882=CARTESIAN_POINT('Origin',(0.27,0.69,-1.3));
#10883=CARTESIAN_POINT('Origin',(0.27,0.69,-1.3));
#10884=CARTESIAN_POINT('',(0.27,0.69,-1.335));
#10885=CARTESIAN_POINT('',(0.,0.,0.));
#10886=CARTESIAN_POINT('Origin',(0.560710678,0.3,-0.955882353));
#10887=CARTESIAN_POINT('',(-0.30000000000004,0.316540540958999,-0.937136406587632));
#10888=CARTESIAN_POINT('',(-0.300000000000018,0.283459459165358,-0.974628299273766));
#10889=CARTESIAN_POINT('Origin',(-0.3,0.300000000061598,-0.955882352930187));
#10890=CARTESIAN_POINT('Origin',(-0.3,0.300000000061598,-0.955882352930187));
#10891=CARTESIAN_POINT('Origin',(-0.3,0.716460202,-1.323347237));
#10892=CARTESIAN_POINT('',(-0.300000000000012,0.70654054091276,-1.28125405363744));
#10893=CARTESIAN_POINT('',(-0.3,0.733000742863165,-1.30460129069508));
#10894=CARTESIAN_POINT('',(-0.300000000000004,0.673459459119238,-1.31874594632367));
#10895=CARTESIAN_POINT('Origin',(-0.3,0.690000000016651,-1.29999999998113));
#10896=CARTESIAN_POINT('Origin',(-0.3,0.690000000016651,-1.29999999998113));
#10897=CARTESIAN_POINT('Origin',(-0.35,0.69,-1.3));
#10898=CARTESIAN_POINT('',(0.,0.,0.));
#10899=CARTESIAN_POINT('Origin',(0.35,0.69,-1.3));
#10900=CARTESIAN_POINT('',(-0.35,0.69,-1.325));
#10901=CARTESIAN_POINT('Origin',(-0.35,0.69,-1.3));
#10902=CARTESIAN_POINT('',(0.35,0.69,-1.325));
#10903=CARTESIAN_POINT('',(0.35,0.69,-1.325));
#10904=CARTESIAN_POINT('Origin',(0.35,0.69,-1.3));
#10905=CARTESIAN_POINT('Origin',(0.35,0.69,-1.3));
#10906=CARTESIAN_POINT('Origin',(-0.35,0.69,-1.3));
#10907=CARTESIAN_POINT('',(1.04512838556094,1.65136027488207,1.86547237816828));
#10908=CARTESIAN_POINT('',(1.04512838556094,1.65136027488207,1.86547237816828));
#10909=CARTESIAN_POINT('',(1.04512838556094,1.65136027488207,1.86547237816828));
#10910=CARTESIAN_POINT('',(1.04512838556094,1.65136027488207,1.86547237816828));
#10911=CARTESIAN_POINT('',(1.04512838556094,1.65136027488207,1.86547237816828));
#10912=CARTESIAN_POINT('',(0.,0.,0.));
#10913=CARTESIAN_POINT('Origin',(-0.46,0.35,1.1));
#10914=CARTESIAN_POINT('',(-0.5,0.35,1.072));
#10915=CARTESIAN_POINT('Origin',(-0.5,0.35,1.1));
#10916=CARTESIAN_POINT('',(-0.46,0.35,1.072));
#10917=CARTESIAN_POINT('',(-0.46,0.35,1.072));
#10918=CARTESIAN_POINT('Origin',(-0.46,0.35,1.1));
#10919=CARTESIAN_POINT('Origin',(-0.46,0.35,1.1));
#10920=CARTESIAN_POINT('',(-0.46,0.35,1.125));
#10921=CARTESIAN_POINT('Origin',(-0.46,0.35,1.1));
#10922=CARTESIAN_POINT('Origin',(-0.5,0.35003431001795,1.0350379192153));
#10923=CARTESIAN_POINT('',(-0.5,0.3,0.92));
#10924=CARTESIAN_POINT('',(-0.500000000000071,0.3,1.10000000002108));
#10925=CARTESIAN_POINT('',(-0.5,0.3,0.92));
#10926=CARTESIAN_POINT('',(-0.5,0.349999999999381,0.92));
#10927=CARTESIAN_POINT('',(-0.5,0.3499999998929,0.919999999999999));
#10928=CARTESIAN_POINT('',(-0.5,0.392836676173592,1.07421203431058));
#10929=CARTESIAN_POINT('Origin',(-0.5,0.649,0.92));
#10930=CARTESIAN_POINT('Origin',(-0.5,0.35,1.1));
#10931=CARTESIAN_POINT('',(-0.5,0.3125,0.985));
#10932=CARTESIAN_POINT('Origin',(-0.5,0.3125,0.98));
#10933=CARTESIAN_POINT('',(-0.5,0.3375,0.945));
#10934=CARTESIAN_POINT('Origin',(-0.5,0.3375,0.94));
#10935=CARTESIAN_POINT('',(-0.5,0.3375,0.985));
#10936=CARTESIAN_POINT('Origin',(-0.5,0.3375,0.98));
#10937=CARTESIAN_POINT('',(-0.5,0.3125,0.945));
#10938=CARTESIAN_POINT('Origin',(-0.5,0.3125,0.94));
#10939=CARTESIAN_POINT('Origin',(-0.51,0.35,1.1));
#10940=CARTESIAN_POINT('',(-0.51,0.35,1.125));
#10941=CARTESIAN_POINT('Origin',(-0.51,0.35,1.1));
#10942=CARTESIAN_POINT('',(-0.51,0.35,1.125));
#10943=CARTESIAN_POINT('Origin',(-0.51,0.3125,0.94));
#10944=CARTESIAN_POINT('',(-0.51,0.3125,0.945));
#10945=CARTESIAN_POINT('Origin',(-0.51,0.3125,0.94));
#10946=CARTESIAN_POINT('',(-0.51,0.3125,0.945));
#10947=CARTESIAN_POINT('Origin',(-0.51,0.3375,0.98));
#10948=CARTESIAN_POINT('',(-0.51,0.3375,0.985));
#10949=CARTESIAN_POINT('Origin',(-0.51,0.3375,0.98));
#10950=CARTESIAN_POINT('',(-0.51,0.3375,0.985));
#10951=CARTESIAN_POINT('Origin',(-0.51,0.3375,0.94));
#10952=CARTESIAN_POINT('',(-0.51,0.3375,0.945));
#10953=CARTESIAN_POINT('Origin',(-0.51,0.3375,0.94));
#10954=CARTESIAN_POINT('',(-0.51,0.3375,0.945));
#10955=CARTESIAN_POINT('Origin',(-0.51,0.3125,0.98));
#10956=CARTESIAN_POINT('',(-0.51,0.3125,0.985));
#10957=CARTESIAN_POINT('Origin',(-0.51,0.3125,0.98));
#10958=CARTESIAN_POINT('',(-0.51,0.3125,0.985));
#10959=CARTESIAN_POINT('Origin',(-0.505,0.325,0.92));
#10960=CARTESIAN_POINT('',(-0.51,0.349999999999358,0.92));
#10961=CARTESIAN_POINT('',(-0.500000000000001,0.35,0.92));
#10962=CARTESIAN_POINT('',(-0.51,0.3,0.92));
#10963=CARTESIAN_POINT('',(-0.510000000000001,0.3,0.92));
#10964=CARTESIAN_POINT('',(-0.510000000000001,0.34999999975,0.92));
#10965=CARTESIAN_POINT('Origin',(-0.51,0.649,0.92));
#10966=CARTESIAN_POINT('',(-0.51,0.392836676173675,1.07421203431072));
#10967=CARTESIAN_POINT('Origin',(-0.51,0.649,0.92));
#10968=CARTESIAN_POINT('',(-0.50999999975,0.392836676172712,1.07421203430912));
#10969=CARTESIAN_POINT('Origin',(-0.51,0.35,1.1));
#10970=CARTESIAN_POINT('',(-0.510000000000001,0.3,1.10000000001774));
#10971=CARTESIAN_POINT('',(-0.50000000025,0.3,1.10000000001923));
#10972=CARTESIAN_POINT('Origin',(-0.51,0.35,1.1));
#10973=CARTESIAN_POINT('Origin',(-0.505,0.3,1.01));
#10974=CARTESIAN_POINT('',(-0.510000000000002,0.3,1.1));
#10975=CARTESIAN_POINT('Origin',(-0.51,0.35003431001795,1.0350379192153));
#10976=CARTESIAN_POINT('',(0.,0.,0.));
#10977=CARTESIAN_POINT('',(0.,0.,0.));
#10978=CARTESIAN_POINT('Origin',(0.595,-0.386547301,0.));
#10979=CARTESIAN_POINT('',(0.595,-0.386547301,-0.025));
#10980=CARTESIAN_POINT('Origin',(0.595,-0.386547301,0.));
#10981=CARTESIAN_POINT('',(0.555,-0.386547301,-0.025));
#10982=CARTESIAN_POINT('',(0.595,-0.386547301,-0.025));
#10983=CARTESIAN_POINT('Origin',(0.555,-0.386547301,0.));
#10984=CARTESIAN_POINT('Origin',(0.555,-0.3865473015,4.16333634234433E-19));
#10985=CARTESIAN_POINT('',(0.555,-0.386547301,-0.174999999));
#10986=CARTESIAN_POINT('Origin',(0.555,-0.386547301,0.));
#10987=CARTESIAN_POINT('Origin',(0.595,-0.3865473015,4.16333634234433E-19));
#10988=CARTESIAN_POINT('',(0.595,-0.386547301,-0.174999999));
#10989=CARTESIAN_POINT('Origin',(0.595,-0.386547301,0.));
#10990=CARTESIAN_POINT('Origin',(0.595,-0.386547301,0.));
#10991=CARTESIAN_POINT('',(0.595,-0.386547301,-0.174999999));
#10992=CARTESIAN_POINT('',(0.,0.,0.));
#10993=CARTESIAN_POINT('Origin',(-0.595,-0.386547301,0.));
#10994=CARTESIAN_POINT('',(-0.595,-0.386547301,0.025));
#10995=CARTESIAN_POINT('Origin',(-0.595,-0.386547301,0.));
#10996=CARTESIAN_POINT('',(-0.555,-0.386547301,0.025));
#10997=CARTESIAN_POINT('',(-0.595,-0.386547301,0.025));
#10998=CARTESIAN_POINT('Origin',(-0.555,-0.386547301,0.));
#10999=CARTESIAN_POINT('Origin',(-0.555,-0.3865473015,4.16333634234433E-19));
#11000=CARTESIAN_POINT('',(-0.555,-0.386547301,0.174999999));
#11001=CARTESIAN_POINT('Origin',(-0.555,-0.386547301,0.));
#11002=CARTESIAN_POINT('Origin',(-0.595,-0.3865473015,4.16333634234433E-19));
#11003=CARTESIAN_POINT('',(-0.595,-0.386547301,0.174999999));
#11004=CARTESIAN_POINT('Origin',(-0.595,-0.386547301,0.));
#11005=CARTESIAN_POINT('Origin',(-0.595,-0.386547301,0.));
#11006=CARTESIAN_POINT('',(-0.595,-0.386547301,0.174999999));
#11007=CARTESIAN_POINT('',(0.,0.,0.));
#11008=CARTESIAN_POINT('Origin',(0.657,-0.386547301,0.));
#11009=CARTESIAN_POINT('',(-0.657,-0.386547301,-0.025));
#11010=CARTESIAN_POINT('Origin',(-0.657,-0.386547301,0.));
#11011=CARTESIAN_POINT('',(0.657,-0.386547301,-0.025));
#11012=CARTESIAN_POINT('',(0.657,-0.386547301,-0.025));
#11013=CARTESIAN_POINT('Origin',(0.657,-0.386547301,0.));
#11014=CARTESIAN_POINT('Origin',(0.657,-0.386547300999999,-2.61943244872498E-18));
#11015=CARTESIAN_POINT('Origin',(-0.657,-0.386547300999999,-2.61943244872498E-18));
#11016=CARTESIAN_POINT('',(1.04512838556093,0.99821155808381,2.14536968366895));
#11017=CARTESIAN_POINT('',(1.04512838556093,0.99821155808381,2.14536968366895));
#11018=CARTESIAN_POINT('',(1.04512838556093,0.99821155808381,2.14536968366895));
#11019=CARTESIAN_POINT('',(0.505128385560943,2.00136027488207,2.96547237816828));
#11020=CARTESIAN_POINT('',(1.51262838556094,2.00136027488207,2.96547237816828));
#11021=CARTESIAN_POINT('',(1.54762838556094,2.00136027488207,2.96547237816828));
#11022=CARTESIAN_POINT('',(0.505128385560942,1.26481297340608,1.86547237816828));
#11023=CARTESIAN_POINT('',(0.50460205538538,1.2648129734061,1.86547237816827));
#11024=CARTESIAN_POINT('',(1.04512838556094,1.65136027488207,1.86547237816828));
#11025=CARTESIAN_POINT('',(0.577628385560944,2.00136027488207,2.96547237816828));
#11026=CARTESIAN_POINT('',(1.04512838556094,1.65136027488208,1.86547237816827));
#11027=CARTESIAN_POINT('',(0.542628385560944,2.00136027488207,2.96547237816828));
#11028=CARTESIAN_POINT('',(0.,0.,0.));
#11029=CARTESIAN_POINT('',(1.04512838556094,1.65136027488207,1.86547237816828));
#11030=CARTESIAN_POINT('',(1.04512838556094,1.66136027488207,1.86547237816828));
#11031=CARTESIAN_POINT('',(0.,0.,0.));
#11032=CARTESIAN_POINT('',(0.,0.,0.));
#11033=CARTESIAN_POINT('',(1.04512838556094,1.65136027488208,1.86547237816827));
#11034=CARTESIAN_POINT('',(0.,0.,0.));
#11035=UNCERTAINTY_MEASURE_WITH_UNIT(LENGTH_MEASURE(1.E-5),#11113,
'DISTANCE_ACCURACY_VALUE',
'Maximum model space distance between geometric entities at asserted c
onnectivities');
#11036=UNCERTAINTY_MEASURE_WITH_UNIT(LENGTH_MEASURE(1.E-5),#11113,
'DISTANCE_ACCURACY_VALUE',
'Maximum model space distance between geometric entities at asserted c
onnectivities');
#11037=UNCERTAINTY_MEASURE_WITH_UNIT(LENGTH_MEASURE(1.E-5),#11113,
'DISTANCE_ACCURACY_VALUE',
'Maximum model space distance between geometric entities at asserted c
onnectivities');
#11038=UNCERTAINTY_MEASURE_WITH_UNIT(LENGTH_MEASURE(1.E-5),#11113,
'DISTANCE_ACCURACY_VALUE',
'Maximum model space distance between geometric entities at asserted c
onnectivities');
#11039=UNCERTAINTY_MEASURE_WITH_UNIT(LENGTH_MEASURE(1.E-5),#11113,
'DISTANCE_ACCURACY_VALUE',
'Maximum model space distance between geometric entities at asserted c
onnectivities');
#11040=UNCERTAINTY_MEASURE_WITH_UNIT(LENGTH_MEASURE(1.E-5),#11113,
'DISTANCE_ACCURACY_VALUE',
'Maximum model space distance between geometric entities at asserted c
onnectivities');
#11041=UNCERTAINTY_MEASURE_WITH_UNIT(LENGTH_MEASURE(1.E-5),#11113,
'DISTANCE_ACCURACY_VALUE',
'Maximum model space distance between geometric entities at asserted c
onnectivities');
#11042=UNCERTAINTY_MEASURE_WITH_UNIT(LENGTH_MEASURE(1.E-5),#11113,
'DISTANCE_ACCURACY_VALUE',
'Maximum model space distance between geometric entities at asserted c
onnectivities');
#11043=UNCERTAINTY_MEASURE_WITH_UNIT(LENGTH_MEASURE(1.E-5),#11113,
'DISTANCE_ACCURACY_VALUE',
'Maximum model space distance between geometric entities at asserted c
onnectivities');
#11044=UNCERTAINTY_MEASURE_WITH_UNIT(LENGTH_MEASURE(1.E-5),#11113,
'DISTANCE_ACCURACY_VALUE',
'Maximum model space distance between geometric entities at asserted c
onnectivities');
#11045=UNCERTAINTY_MEASURE_WITH_UNIT(LENGTH_MEASURE(1.E-5),#11113,
'DISTANCE_ACCURACY_VALUE',
'Maximum model space distance between geometric entities at asserted c
onnectivities');
#11046=UNCERTAINTY_MEASURE_WITH_UNIT(LENGTH_MEASURE(1.E-5),#11113,
'DISTANCE_ACCURACY_VALUE',
'Maximum model space distance between geometric entities at asserted c
onnectivities');
#11047=UNCERTAINTY_MEASURE_WITH_UNIT(LENGTH_MEASURE(1.E-5),#11113,
'DISTANCE_ACCURACY_VALUE',
'Maximum model space distance between geometric entities at asserted c
onnectivities');
#11048=UNCERTAINTY_MEASURE_WITH_UNIT(LENGTH_MEASURE(1.E-5),#11113,
'DISTANCE_ACCURACY_VALUE',
'Maximum model space distance between geometric entities at asserted c
onnectivities');
#11049=UNCERTAINTY_MEASURE_WITH_UNIT(LENGTH_MEASURE(1.E-5),#11113,
'DISTANCE_ACCURACY_VALUE',
'Maximum model space distance between geometric entities at asserted c
onnectivities');
#11050=UNCERTAINTY_MEASURE_WITH_UNIT(LENGTH_MEASURE(1.E-5),#11113,
'DISTANCE_ACCURACY_VALUE',
'Maximum model space distance between geometric entities at asserted c
onnectivities');
#11051=UNCERTAINTY_MEASURE_WITH_UNIT(LENGTH_MEASURE(1.E-5),#11113,
'DISTANCE_ACCURACY_VALUE',
'Maximum model space distance between geometric entities at asserted c
onnectivities');
#11052=UNCERTAINTY_MEASURE_WITH_UNIT(LENGTH_MEASURE(1.E-5),#11113,
'DISTANCE_ACCURACY_VALUE',
'Maximum model space distance between geometric entities at asserted c
onnectivities');
#11053=UNCERTAINTY_MEASURE_WITH_UNIT(LENGTH_MEASURE(1.E-5),#11113,
'DISTANCE_ACCURACY_VALUE',
'Maximum model space distance between geometric entities at asserted c
onnectivities');
#11054=UNCERTAINTY_MEASURE_WITH_UNIT(LENGTH_MEASURE(1.E-5),#11113,
'DISTANCE_ACCURACY_VALUE',
'Maximum model space distance between geometric entities at asserted c
onnectivities');
#11055=UNCERTAINTY_MEASURE_WITH_UNIT(LENGTH_MEASURE(1.E-5),#11113,
'DISTANCE_ACCURACY_VALUE',
'Maximum model space distance between geometric entities at asserted c
onnectivities');
#11056=UNCERTAINTY_MEASURE_WITH_UNIT(LENGTH_MEASURE(1.E-5),#11113,
'DISTANCE_ACCURACY_VALUE',
'Maximum model space distance between geometric entities at asserted c
onnectivities');
#11057=UNCERTAINTY_MEASURE_WITH_UNIT(LENGTH_MEASURE(1.E-5),#11113,
'DISTANCE_ACCURACY_VALUE',
'Maximum model space distance between geometric entities at asserted c
onnectivities');
#11058=UNCERTAINTY_MEASURE_WITH_UNIT(LENGTH_MEASURE(1.E-5),#11113,
'DISTANCE_ACCURACY_VALUE',
'Maximum model space distance between geometric entities at asserted c
onnectivities');
#11059=UNCERTAINTY_MEASURE_WITH_UNIT(LENGTH_MEASURE(1.E-5),#11113,
'DISTANCE_ACCURACY_VALUE',
'Maximum model space distance between geometric entities at asserted c
onnectivities');
#11060=UNCERTAINTY_MEASURE_WITH_UNIT(LENGTH_MEASURE(1.E-5),#11113,
'DISTANCE_ACCURACY_VALUE',
'Maximum model space distance between geometric entities at asserted c
onnectivities');
#11061=UNCERTAINTY_MEASURE_WITH_UNIT(LENGTH_MEASURE(1.E-5),#11113,
'DISTANCE_ACCURACY_VALUE',
'Maximum model space distance between geometric entities at asserted c
onnectivities');
#11062=UNCERTAINTY_MEASURE_WITH_UNIT(LENGTH_MEASURE(1.E-5),#11113,
'DISTANCE_ACCURACY_VALUE',
'Maximum model space distance between geometric entities at asserted c
onnectivities');
#11063=UNCERTAINTY_MEASURE_WITH_UNIT(LENGTH_MEASURE(1.E-5),#11113,
'DISTANCE_ACCURACY_VALUE',
'Maximum model space distance between geometric entities at asserted c
onnectivities');
#11064=UNCERTAINTY_MEASURE_WITH_UNIT(LENGTH_MEASURE(1.E-5),#11113,
'DISTANCE_ACCURACY_VALUE',
'Maximum model space distance between geometric entities at asserted c
onnectivities');
#11065=UNCERTAINTY_MEASURE_WITH_UNIT(LENGTH_MEASURE(1.E-5),#11113,
'DISTANCE_ACCURACY_VALUE',
'Maximum model space distance between geometric entities at asserted c
onnectivities');
#11066=UNCERTAINTY_MEASURE_WITH_UNIT(LENGTH_MEASURE(1.E-5),#11113,
'DISTANCE_ACCURACY_VALUE',
'Maximum model space distance between geometric entities at asserted c
onnectivities');
#11067=UNCERTAINTY_MEASURE_WITH_UNIT(LENGTH_MEASURE(1.E-5),#11113,
'DISTANCE_ACCURACY_VALUE',
'Maximum model space distance between geometric entities at asserted c
onnectivities');
#11068=UNCERTAINTY_MEASURE_WITH_UNIT(LENGTH_MEASURE(1.E-5),#11113,
'DISTANCE_ACCURACY_VALUE',
'Maximum model space distance between geometric entities at asserted c
onnectivities');
#11069=UNCERTAINTY_MEASURE_WITH_UNIT(LENGTH_MEASURE(1.E-5),#11113,
'DISTANCE_ACCURACY_VALUE',
'Maximum model space distance between geometric entities at asserted c
onnectivities');
#11070=UNCERTAINTY_MEASURE_WITH_UNIT(LENGTH_MEASURE(1.E-5),#11113,
'DISTANCE_ACCURACY_VALUE',
'Maximum model space distance between geometric entities at asserted c
onnectivities');
#11071=UNCERTAINTY_MEASURE_WITH_UNIT(LENGTH_MEASURE(1.E-5),#11113,
'DISTANCE_ACCURACY_VALUE',
'Maximum model space distance between geometric entities at asserted c
onnectivities');
#11072=UNCERTAINTY_MEASURE_WITH_UNIT(LENGTH_MEASURE(1.E-5),#11113,
'DISTANCE_ACCURACY_VALUE',
'Maximum model space distance between geometric entities at asserted c
onnectivities');
#11073=UNCERTAINTY_MEASURE_WITH_UNIT(LENGTH_MEASURE(1.E-5),#11113,
'DISTANCE_ACCURACY_VALUE',
'Maximum model space distance between geometric entities at asserted c
onnectivities');
#11074=(
GEOMETRIC_REPRESENTATION_CONTEXT(3)
GLOBAL_UNCERTAINTY_ASSIGNED_CONTEXT((#11035))
GLOBAL_UNIT_ASSIGNED_CONTEXT((#11113,#11114,#11115))
REPRESENTATION_CONTEXT('','3D')
);
#11075=(
GEOMETRIC_REPRESENTATION_CONTEXT(3)
GLOBAL_UNCERTAINTY_ASSIGNED_CONTEXT((#11036))
GLOBAL_UNIT_ASSIGNED_CONTEXT((#11113,#11114,#11115))
REPRESENTATION_CONTEXT('','3D')
);
#11076=(
GEOMETRIC_REPRESENTATION_CONTEXT(3)
GLOBAL_UNCERTAINTY_ASSIGNED_CONTEXT((#11037))
GLOBAL_UNIT_ASSIGNED_CONTEXT((#11113,#11114,#11115))
REPRESENTATION_CONTEXT('','3D')
);
#11077=(
GEOMETRIC_REPRESENTATION_CONTEXT(3)
GLOBAL_UNCERTAINTY_ASSIGNED_CONTEXT((#11038))
GLOBAL_UNIT_ASSIGNED_CONTEXT((#11113,#11114,#11115))
REPRESENTATION_CONTEXT('','3D')
);
#11078=(
GEOMETRIC_REPRESENTATION_CONTEXT(3)
GLOBAL_UNCERTAINTY_ASSIGNED_CONTEXT((#11039))
GLOBAL_UNIT_ASSIGNED_CONTEXT((#11113,#11114,#11115))
REPRESENTATION_CONTEXT('','3D')
);
#11079=(
GEOMETRIC_REPRESENTATION_CONTEXT(3)
GLOBAL_UNCERTAINTY_ASSIGNED_CONTEXT((#11040))
GLOBAL_UNIT_ASSIGNED_CONTEXT((#11113,#11114,#11115))
REPRESENTATION_CONTEXT('','3D')
);
#11080=(
GEOMETRIC_REPRESENTATION_CONTEXT(3)
GLOBAL_UNCERTAINTY_ASSIGNED_CONTEXT((#11041))
GLOBAL_UNIT_ASSIGNED_CONTEXT((#11113,#11114,#11115))
REPRESENTATION_CONTEXT('','3D')
);
#11081=(
GEOMETRIC_REPRESENTATION_CONTEXT(3)
GLOBAL_UNCERTAINTY_ASSIGNED_CONTEXT((#11042))
GLOBAL_UNIT_ASSIGNED_CONTEXT((#11113,#11114,#11115))
REPRESENTATION_CONTEXT('','3D')
);
#11082=(
GEOMETRIC_REPRESENTATION_CONTEXT(3)
GLOBAL_UNCERTAINTY_ASSIGNED_CONTEXT((#11043))
GLOBAL_UNIT_ASSIGNED_CONTEXT((#11113,#11114,#11115))
REPRESENTATION_CONTEXT('','3D')
);
#11083=(
GEOMETRIC_REPRESENTATION_CONTEXT(3)
GLOBAL_UNCERTAINTY_ASSIGNED_CONTEXT((#11044))
GLOBAL_UNIT_ASSIGNED_CONTEXT((#11113,#11114,#11115))
REPRESENTATION_CONTEXT('','3D')
);
#11084=(
GEOMETRIC_REPRESENTATION_CONTEXT(3)
GLOBAL_UNCERTAINTY_ASSIGNED_CONTEXT((#11045))
GLOBAL_UNIT_ASSIGNED_CONTEXT((#11113,#11114,#11115))
REPRESENTATION_CONTEXT('','3D')
);
#11085=(
GEOMETRIC_REPRESENTATION_CONTEXT(3)
GLOBAL_UNCERTAINTY_ASSIGNED_CONTEXT((#11046))
GLOBAL_UNIT_ASSIGNED_CONTEXT((#11113,#11114,#11115))
REPRESENTATION_CONTEXT('','3D')
);
#11086=(
GEOMETRIC_REPRESENTATION_CONTEXT(3)
GLOBAL_UNCERTAINTY_ASSIGNED_CONTEXT((#11047))
GLOBAL_UNIT_ASSIGNED_CONTEXT((#11113,#11114,#11115))
REPRESENTATION_CONTEXT('','3D')
);
#11087=(
GEOMETRIC_REPRESENTATION_CONTEXT(3)
GLOBAL_UNCERTAINTY_ASSIGNED_CONTEXT((#11048))
GLOBAL_UNIT_ASSIGNED_CONTEXT((#11113,#11114,#11115))
REPRESENTATION_CONTEXT('','3D')
);
#11088=(
GEOMETRIC_REPRESENTATION_CONTEXT(3)
GLOBAL_UNCERTAINTY_ASSIGNED_CONTEXT((#11049))
GLOBAL_UNIT_ASSIGNED_CONTEXT((#11113,#11114,#11115))
REPRESENTATION_CONTEXT('','3D')
);
#11089=(
GEOMETRIC_REPRESENTATION_CONTEXT(3)
GLOBAL_UNCERTAINTY_ASSIGNED_CONTEXT((#11050))
GLOBAL_UNIT_ASSIGNED_CONTEXT((#11113,#11114,#11115))
REPRESENTATION_CONTEXT('','3D')
);
#11090=(
GEOMETRIC_REPRESENTATION_CONTEXT(3)
GLOBAL_UNCERTAINTY_ASSIGNED_CONTEXT((#11051))
GLOBAL_UNIT_ASSIGNED_CONTEXT((#11113,#11114,#11115))
REPRESENTATION_CONTEXT('','3D')
);
#11091=(
GEOMETRIC_REPRESENTATION_CONTEXT(3)
GLOBAL_UNCERTAINTY_ASSIGNED_CONTEXT((#11052))
GLOBAL_UNIT_ASSIGNED_CONTEXT((#11113,#11114,#11115))
REPRESENTATION_CONTEXT('','3D')
);
#11092=(
GEOMETRIC_REPRESENTATION_CONTEXT(3)
GLOBAL_UNCERTAINTY_ASSIGNED_CONTEXT((#11053))
GLOBAL_UNIT_ASSIGNED_CONTEXT((#11113,#11114,#11115))
REPRESENTATION_CONTEXT('','3D')
);
#11093=(
GEOMETRIC_REPRESENTATION_CONTEXT(3)
GLOBAL_UNCERTAINTY_ASSIGNED_CONTEXT((#11054))
GLOBAL_UNIT_ASSIGNED_CONTEXT((#11113,#11114,#11115))
REPRESENTATION_CONTEXT('','3D')
);
#11094=(
GEOMETRIC_REPRESENTATION_CONTEXT(3)
GLOBAL_UNCERTAINTY_ASSIGNED_CONTEXT((#11055))
GLOBAL_UNIT_ASSIGNED_CONTEXT((#11113,#11114,#11115))
REPRESENTATION_CONTEXT('','3D')
);
#11095=(
GEOMETRIC_REPRESENTATION_CONTEXT(3)
GLOBAL_UNCERTAINTY_ASSIGNED_CONTEXT((#11056))
GLOBAL_UNIT_ASSIGNED_CONTEXT((#11113,#11114,#11115))
REPRESENTATION_CONTEXT('','3D')
);
#11096=(
GEOMETRIC_REPRESENTATION_CONTEXT(3)
GLOBAL_UNCERTAINTY_ASSIGNED_CONTEXT((#11057))
GLOBAL_UNIT_ASSIGNED_CONTEXT((#11113,#11114,#11115))
REPRESENTATION_CONTEXT('','3D')
);
#11097=(
GEOMETRIC_REPRESENTATION_CONTEXT(3)
GLOBAL_UNCERTAINTY_ASSIGNED_CONTEXT((#11058))
GLOBAL_UNIT_ASSIGNED_CONTEXT((#11113,#11114,#11115))
REPRESENTATION_CONTEXT('','3D')
);
#11098=(
GEOMETRIC_REPRESENTATION_CONTEXT(3)
GLOBAL_UNCERTAINTY_ASSIGNED_CONTEXT((#11059))
GLOBAL_UNIT_ASSIGNED_CONTEXT((#11113,#11114,#11115))
REPRESENTATION_CONTEXT('','3D')
);
#11099=(
GEOMETRIC_REPRESENTATION_CONTEXT(3)
GLOBAL_UNCERTAINTY_ASSIGNED_CONTEXT((#11060))
GLOBAL_UNIT_ASSIGNED_CONTEXT((#11113,#11114,#11115))
REPRESENTATION_CONTEXT('','3D')
);
#11100=(
GEOMETRIC_REPRESENTATION_CONTEXT(3)
GLOBAL_UNCERTAINTY_ASSIGNED_CONTEXT((#11061))
GLOBAL_UNIT_ASSIGNED_CONTEXT((#11113,#11114,#11115))
REPRESENTATION_CONTEXT('','3D')
);
#11101=(
GEOMETRIC_REPRESENTATION_CONTEXT(3)
GLOBAL_UNCERTAINTY_ASSIGNED_CONTEXT((#11062))
GLOBAL_UNIT_ASSIGNED_CONTEXT((#11113,#11114,#11115))
REPRESENTATION_CONTEXT('','3D')
);
#11102=(
GEOMETRIC_REPRESENTATION_CONTEXT(3)
GLOBAL_UNCERTAINTY_ASSIGNED_CONTEXT((#11063))
GLOBAL_UNIT_ASSIGNED_CONTEXT((#11113,#11114,#11115))
REPRESENTATION_CONTEXT('','3D')
);
#11103=(
GEOMETRIC_REPRESENTATION_CONTEXT(3)
GLOBAL_UNCERTAINTY_ASSIGNED_CONTEXT((#11064))
GLOBAL_UNIT_ASSIGNED_CONTEXT((#11113,#11114,#11115))
REPRESENTATION_CONTEXT('','3D')
);
#11104=(
GEOMETRIC_REPRESENTATION_CONTEXT(3)
GLOBAL_UNCERTAINTY_ASSIGNED_CONTEXT((#11065))
GLOBAL_UNIT_ASSIGNED_CONTEXT((#11113,#11114,#11115))
REPRESENTATION_CONTEXT('','3D')
);
#11105=(
GEOMETRIC_REPRESENTATION_CONTEXT(3)
GLOBAL_UNCERTAINTY_ASSIGNED_CONTEXT((#11066))
GLOBAL_UNIT_ASSIGNED_CONTEXT((#11113,#11114,#11115))
REPRESENTATION_CONTEXT('','3D')
);
#11106=(
GEOMETRIC_REPRESENTATION_CONTEXT(3)
GLOBAL_UNCERTAINTY_ASSIGNED_CONTEXT((#11067))
GLOBAL_UNIT_ASSIGNED_CONTEXT((#11113,#11114,#11115))
REPRESENTATION_CONTEXT('','3D')
);
#11107=(
GEOMETRIC_REPRESENTATION_CONTEXT(3)
GLOBAL_UNCERTAINTY_ASSIGNED_CONTEXT((#11068))
GLOBAL_UNIT_ASSIGNED_CONTEXT((#11113,#11114,#11115))
REPRESENTATION_CONTEXT('','3D')
);
#11108=(
GEOMETRIC_REPRESENTATION_CONTEXT(3)
GLOBAL_UNCERTAINTY_ASSIGNED_CONTEXT((#11069))
GLOBAL_UNIT_ASSIGNED_CONTEXT((#11113,#11114,#11115))
REPRESENTATION_CONTEXT('','3D')
);
#11109=(
GEOMETRIC_REPRESENTATION_CONTEXT(3)
GLOBAL_UNCERTAINTY_ASSIGNED_CONTEXT((#11070))
GLOBAL_UNIT_ASSIGNED_CONTEXT((#11113,#11114,#11115))
REPRESENTATION_CONTEXT('','3D')
);
#11110=(
GEOMETRIC_REPRESENTATION_CONTEXT(3)
GLOBAL_UNCERTAINTY_ASSIGNED_CONTEXT((#11071))
GLOBAL_UNIT_ASSIGNED_CONTEXT((#11113,#11114,#11115))
REPRESENTATION_CONTEXT('','3D')
);
#11111=(
GEOMETRIC_REPRESENTATION_CONTEXT(3)
GLOBAL_UNCERTAINTY_ASSIGNED_CONTEXT((#11072))
GLOBAL_UNIT_ASSIGNED_CONTEXT((#11113,#11114,#11115))
REPRESENTATION_CONTEXT('','3D')
);
#11112=(
GEOMETRIC_REPRESENTATION_CONTEXT(3)
GLOBAL_UNCERTAINTY_ASSIGNED_CONTEXT((#11073))
GLOBAL_UNIT_ASSIGNED_CONTEXT((#11113,#11114,#11115))
REPRESENTATION_CONTEXT('','3D')
);
#11113=(
LENGTH_UNIT()
NAMED_UNIT(*)
SI_UNIT($,.METRE.)
);
#11114=(
NAMED_UNIT(*)
PLANE_ANGLE_UNIT()
SI_UNIT($,.RADIAN.)
);
#11115=(
NAMED_UNIT(*)
SI_UNIT($,.STERADIAN.)
SOLID_ANGLE_UNIT()
);
#11116=SHAPE_DEFINITION_REPRESENTATION(#11154,#11229);
#11117=SHAPE_DEFINITION_REPRESENTATION(#11155,#11230);
#11118=SHAPE_DEFINITION_REPRESENTATION(#11156,#11231);
#11119=SHAPE_DEFINITION_REPRESENTATION(#11157,#11232);
#11120=SHAPE_DEFINITION_REPRESENTATION(#11158,#11233);
#11121=SHAPE_DEFINITION_REPRESENTATION(#11159,#11234);
#11122=SHAPE_DEFINITION_REPRESENTATION(#11160,#11235);
#11123=SHAPE_DEFINITION_REPRESENTATION(#11161,#11236);
#11124=SHAPE_DEFINITION_REPRESENTATION(#11162,#11237);
#11125=SHAPE_DEFINITION_REPRESENTATION(#11163,#11238);
#11126=SHAPE_DEFINITION_REPRESENTATION(#11164,#11239);
#11127=SHAPE_DEFINITION_REPRESENTATION(#11165,#11240);
#11128=SHAPE_DEFINITION_REPRESENTATION(#11166,#11241);
#11129=SHAPE_DEFINITION_REPRESENTATION(#11167,#11242);
#11130=SHAPE_DEFINITION_REPRESENTATION(#11168,#11243);
#11131=SHAPE_DEFINITION_REPRESENTATION(#11169,#11244);
#11132=SHAPE_DEFINITION_REPRESENTATION(#11170,#11245);
#11133=SHAPE_DEFINITION_REPRESENTATION(#11171,#11246);
#11134=SHAPE_DEFINITION_REPRESENTATION(#11179,#11247);
#11135=SHAPE_DEFINITION_REPRESENTATION(#11180,#11248);
#11136=SHAPE_DEFINITION_REPRESENTATION(#11181,#11249);
#11137=SHAPE_DEFINITION_REPRESENTATION(#11182,#11250);
#11138=SHAPE_DEFINITION_REPRESENTATION(#11183,#11251);
#11139=SHAPE_DEFINITION_REPRESENTATION(#11184,#11252);
#11140=SHAPE_DEFINITION_REPRESENTATION(#11185,#11253);
#11141=SHAPE_DEFINITION_REPRESENTATION(#11186,#11254);
#11142=SHAPE_DEFINITION_REPRESENTATION(#11187,#11255);
#11143=SHAPE_DEFINITION_REPRESENTATION(#11194,#11256);
#11144=SHAPE_DEFINITION_REPRESENTATION(#11195,#11257);
#11145=SHAPE_DEFINITION_REPRESENTATION(#11196,#11258);
#11146=SHAPE_DEFINITION_REPRESENTATION(#11197,#11259);
#11147=SHAPE_DEFINITION_REPRESENTATION(#11198,#11260);
#11148=SHAPE_DEFINITION_REPRESENTATION(#11199,#11261);
#11149=SHAPE_DEFINITION_REPRESENTATION(#11205,#11262);
#11150=SHAPE_DEFINITION_REPRESENTATION(#11206,#11263);
#11151=SHAPE_DEFINITION_REPRESENTATION(#11207,#11264);
#11152=SHAPE_DEFINITION_REPRESENTATION(#11208,#11265);
#11153=SHAPE_DEFINITION_REPRESENTATION(#11209,#11266);
#11154=PRODUCT_DEFINITION_SHAPE('',$,#11268);
#11155=PRODUCT_DEFINITION_SHAPE('',$,#11269);
#11156=PRODUCT_DEFINITION_SHAPE('',$,#11270);
#11157=PRODUCT_DEFINITION_SHAPE('',$,#11271);
#11158=PRODUCT_DEFINITION_SHAPE('',$,#11272);
#11159=PRODUCT_DEFINITION_SHAPE('',$,#11273);
#11160=PRODUCT_DEFINITION_SHAPE('',$,#11274);
#11161=PRODUCT_DEFINITION_SHAPE('',$,#11275);
#11162=PRODUCT_DEFINITION_SHAPE('',$,#11276);
#11163=PRODUCT_DEFINITION_SHAPE('',$,#11277);
#11164=PRODUCT_DEFINITION_SHAPE('',$,#11278);
#11165=PRODUCT_DEFINITION_SHAPE('',$,#11279);
#11166=PRODUCT_DEFINITION_SHAPE('',$,#11280);
#11167=PRODUCT_DEFINITION_SHAPE('',$,#11281);
#11168=PRODUCT_DEFINITION_SHAPE('',$,#11282);
#11169=PRODUCT_DEFINITION_SHAPE('',$,#11283);
#11170=PRODUCT_DEFINITION_SHAPE('',$,#11284);
#11171=PRODUCT_DEFINITION_SHAPE('',$,#11285);
#11172=PRODUCT_DEFINITION_SHAPE($,$,#130);
#11173=PRODUCT_DEFINITION_SHAPE($,$,#131);
#11174=PRODUCT_DEFINITION_SHAPE($,$,#132);
#11175=PRODUCT_DEFINITION_SHAPE($,$,#133);
#11176=PRODUCT_DEFINITION_SHAPE($,$,#134);
#11177=PRODUCT_DEFINITION_SHAPE($,$,#135);
#11178=PRODUCT_DEFINITION_SHAPE($,$,#136);
#11179=PRODUCT_DEFINITION_SHAPE('',$,#11286);
#11180=PRODUCT_DEFINITION_SHAPE('',$,#11287);
#11181=PRODUCT_DEFINITION_SHAPE('',$,#11288);
#11182=PRODUCT_DEFINITION_SHAPE('',$,#11289);
#11183=PRODUCT_DEFINITION_SHAPE('',$,#11290);
#11184=PRODUCT_DEFINITION_SHAPE('',$,#11291);
#11185=PRODUCT_DEFINITION_SHAPE('',$,#11292);
#11186=PRODUCT_DEFINITION_SHAPE('',$,#11293);
#11187=PRODUCT_DEFINITION_SHAPE('',$,#11294);
#11188=PRODUCT_DEFINITION_SHAPE($,$,#137);
#11189=PRODUCT_DEFINITION_SHAPE($,$,#138);
#11190=PRODUCT_DEFINITION_SHAPE($,$,#139);
#11191=PRODUCT_DEFINITION_SHAPE($,$,#140);
#11192=PRODUCT_DEFINITION_SHAPE($,$,#141);
#11193=PRODUCT_DEFINITION_SHAPE($,$,#142);
#11194=PRODUCT_DEFINITION_SHAPE('',$,#11295);
#11195=PRODUCT_DEFINITION_SHAPE('',$,#11296);
#11196=PRODUCT_DEFINITION_SHAPE('',$,#11297);
#11197=PRODUCT_DEFINITION_SHAPE('',$,#11298);
#11198=PRODUCT_DEFINITION_SHAPE('',$,#11299);
#11199=PRODUCT_DEFINITION_SHAPE('',$,#11300);
#11200=PRODUCT_DEFINITION_SHAPE($,$,#143);
#11201=PRODUCT_DEFINITION_SHAPE($,$,#144);
#11202=PRODUCT_DEFINITION_SHAPE($,$,#145);
#11203=PRODUCT_DEFINITION_SHAPE($,$,#146);
#11204=PRODUCT_DEFINITION_SHAPE($,$,#147);
#11205=PRODUCT_DEFINITION_SHAPE('',$,#11301);
#11206=PRODUCT_DEFINITION_SHAPE('',$,#11302);
#11207=PRODUCT_DEFINITION_SHAPE('',$,#11303);
#11208=PRODUCT_DEFINITION_SHAPE('',$,#11304);
#11209=PRODUCT_DEFINITION_SHAPE('',$,#11305);
#11210=PRODUCT_DEFINITION_SHAPE($,$,#148);
#11211=PRODUCT_DEFINITION_SHAPE($,$,#149);
#11212=PRODUCT_DEFINITION_SHAPE($,$,#150);
#11213=PRODUCT_DEFINITION_SHAPE($,$,#151);
#11214=PRODUCT_DEFINITION_SHAPE($,$,#152);
#11215=PRODUCT_DEFINITION_SHAPE($,$,#153);
#11216=PRODUCT_DEFINITION_SHAPE($,$,#154);
#11217=PRODUCT_DEFINITION_SHAPE($,$,#155);
#11218=PRODUCT_DEFINITION_SHAPE($,$,#156);
#11219=PRODUCT_DEFINITION_SHAPE($,$,#157);
#11220=PRODUCT_DEFINITION_SHAPE($,$,#158);
#11221=PRODUCT_DEFINITION_SHAPE($,$,#159);
#11222=PRODUCT_DEFINITION_SHAPE($,$,#160);
#11223=PRODUCT_DEFINITION_SHAPE($,$,#161);
#11224=PRODUCT_DEFINITION_SHAPE($,$,#162);
#11225=PRODUCT_DEFINITION_SHAPE($,$,#163);
#11226=PRODUCT_DEFINITION_SHAPE($,$,#164);
#11227=PRODUCT_DEFINITION_SHAPE($,$,#165);
#11228=PRODUCT_DEFINITION_SHAPE($,$,#166);
#11229=SHAPE_REPRESENTATION('',(#6407,#7244,#7245,#7246,#7247,#7248,#7249,
#7250,#7251,#7252,#7253,#7254,#7255,#7256,#7257,#7258,#7259),#11074);
#11230=SHAPE_REPRESENTATION('',(#6408),#11075);
#11231=SHAPE_REPRESENTATION('',(#6461),#11076);
#11232=SHAPE_REPRESENTATION('',(#6520),#11077);
#11233=SHAPE_REPRESENTATION('',(#6579),#11078);
#11234=SHAPE_REPRESENTATION('',(#6632),#11079);
#11235=SHAPE_REPRESENTATION('',(#6657),#11080);
#11236=SHAPE_REPRESENTATION('',(#6679),#11081);
#11237=SHAPE_REPRESENTATION('',(#6738),#11082);
#11238=SHAPE_REPRESENTATION('',(#6768),#11083);
#11239=SHAPE_REPRESENTATION('',(#6827,#6954,#6955,#6956,#6957,#6958,#6959,
#6960),#11084);
#11240=SHAPE_REPRESENTATION('',(#6828),#11085);
#11241=SHAPE_REPRESENTATION('',(#6838),#11086);
#11242=SHAPE_REPRESENTATION('',(#6860),#11087);
#11243=SHAPE_REPRESENTATION('',(#6870),#11088);
#11244=SHAPE_REPRESENTATION('',(#6892),#11089);
#11245=SHAPE_REPRESENTATION('',(#6914),#11090);
#11246=SHAPE_REPRESENTATION('',(#6924),#11091);
#11247=SHAPE_REPRESENTATION('',(#6961),#11092);
#11248=SHAPE_REPRESENTATION('',(#7030),#11093);
#11249=SHAPE_REPRESENTATION('',(#7044,#7137,#7138,#7139,#7140,#7141,#7142),
#11094);
#11250=SHAPE_REPRESENTATION('',(#7045),#11095);
#11251=SHAPE_REPRESENTATION('',(#7060),#11096);
#11252=SHAPE_REPRESENTATION('',(#7067),#11097);
#11253=SHAPE_REPRESENTATION('',(#7082),#11098);
#11254=SHAPE_REPRESENTATION('',(#7107),#11099);
#11255=SHAPE_REPRESENTATION('',(#7122),#11100);
#11256=SHAPE_REPRESENTATION('',(#7143,#7181,#7182,#7183,#7184,#7185),#11101);
#11257=SHAPE_REPRESENTATION('',(#7144),#11102);
#11258=SHAPE_REPRESENTATION('',(#7152),#11103);
#11259=SHAPE_REPRESENTATION('',(#7158),#11104);
#11260=SHAPE_REPRESENTATION('',(#7167),#11105);
#11261=SHAPE_REPRESENTATION('',(#7175),#11106);
#11262=SHAPE_REPRESENTATION('',(#7186),#11107);
#11263=SHAPE_REPRESENTATION('',(#7216,#7241,#7242,#7243),#11108);
#11264=SHAPE_REPRESENTATION('',(#7217),#11109);
#11265=SHAPE_REPRESENTATION('',(#7226),#11110);
#11266=SHAPE_REPRESENTATION('',(#7235),#11111);
#11267=PRODUCT_DEFINITION_CONTEXT('part definition',#11383,'design');
#11268=PRODUCT_DEFINITION('MAT-063',
'MAT-063',#11306,#11267);
#11269=PRODUCT_DEFINITION('Pulley Wheel 1','Pulley Wheel 1',#11307,#11267);
#11270=PRODUCT_DEFINITION('Radial Ball Bearing 1',
'Radial Ball Bearing 1',#11308,#11267);
#11271=PRODUCT_DEFINITION('Radial Ball Bearing 2',
'Radial Ball Bearing 2',#11309,#11267);
#11272=PRODUCT_DEFINITION('Pulley Wheel 2','Pulley Wheel 2',#11310,#11267);
#11273=PRODUCT_DEFINITION('Belt','Belt',#11311,#11267);
#11274=PRODUCT_DEFINITION('Wheel Support','Wheel Support',#11312,#11267);
#11275=PRODUCT_DEFINITION('Radial Ball Bearing 3',
'Radial Ball Bearing 3',#11313,#11267);
#11276=PRODUCT_DEFINITION('Mirror Front Support','Mirror Front Support',
#11314,#11267);
#11277=PRODUCT_DEFINITION('Radial Ball Bearing 4',
'Radial Ball Bearing 4',#11315,#11267);
#11278=PRODUCT_DEFINITION('Broom Roller Assembly',
'Broom Roller Assembly',#11316,#11267);
#11279=PRODUCT_DEFINITION('Broom Roller 1','Broom Roller 1',#11317,#11267);
#11280=PRODUCT_DEFINITION('Broom Roller 2','Broom Roller 2',#11318,#11267);
#11281=PRODUCT_DEFINITION('Broom Roller 3','Broom Roller 3',#11319,#11267);
#11282=PRODUCT_DEFINITION('Broom Roller 4','Broom Roller 4',#11320,#11267);
#11283=PRODUCT_DEFINITION('Broom Roller 5','Broom Roller 5',#11321,#11267);
#11284=PRODUCT_DEFINITION('Broom Roller 6','Broom Roller 6',#11322,#11267);
#11285=PRODUCT_DEFINITION('Broom Roller 7','Broom Roller 7',#11323,#11267);
#11286=PRODUCT_DEFINITION('Body','Body',#11324,#11267);
#11287=PRODUCT_DEFINITION('Ground Roller','Ground Roller',#11325,#11267);
#11288=PRODUCT_DEFINITION('Plate Assembly','Plate Assembly',#11326,#11267);
#11289=PRODUCT_DEFINITION('Plate 1','Plate 1',#11327,#11267);
#11290=PRODUCT_DEFINITION('Plate 2','Plate 2',#11328,#11267);
#11291=PRODUCT_DEFINITION('Plate 3','Plate 3',#11329,#11267);
#11292=PRODUCT_DEFINITION('Plate 4','Plate 4',#11330,#11267);
#11293=PRODUCT_DEFINITION('Plate 5','Plate 5',#11331,#11267);
#11294=PRODUCT_DEFINITION('Plate 6','Plate 6',#11332,#11267);
#11295=PRODUCT_DEFINITION('Push Handle Assembly','Push Handle Assembly',
#11333,#11267);
#11296=PRODUCT_DEFINITION('Push Handle 1','Push Handle 1',#11334,#11267);
#11297=PRODUCT_DEFINITION('Push Handle 2','Push Handle 2',#11335,#11267);
#11298=PRODUCT_DEFINITION('Push Handle 3','Push Handle 3',#11336,#11267);
#11299=PRODUCT_DEFINITION('Push Handle 4','Push Handle 4',#11337,#11267);
#11300=PRODUCT_DEFINITION('Push Handle 5','Push Handle 5',#11338,#11267);
#11301=PRODUCT_DEFINITION('Front Support','Front Support',#11339,#11267);
#11302=PRODUCT_DEFINITION('Wheel Assembly','Wheel Assembly',#11340,#11267);
#11303=PRODUCT_DEFINITION('Wheel 1','Wheel 1',#11341,#11267);
#11304=PRODUCT_DEFINITION('Wheel 2','Wheel 2',#11342,#11267);
#11305=PRODUCT_DEFINITION('Wheel 3','Wheel 3',#11343,#11267);
#11306=PRODUCT_DEFINITION_FORMATION('',$,#11385);
#11307=PRODUCT_DEFINITION_FORMATION('',$,#11386);
#11308=PRODUCT_DEFINITION_FORMATION('',$,#11387);
#11309=PRODUCT_DEFINITION_FORMATION('',$,#11388);
#11310=PRODUCT_DEFINITION_FORMATION('',$,#11389);
#11311=PRODUCT_DEFINITION_FORMATION('',$,#11390);
#11312=PRODUCT_DEFINITION_FORMATION('',$,#11391);
#11313=PRODUCT_DEFINITION_FORMATION('',$,#11392);
#11314=PRODUCT_DEFINITION_FORMATION('',$,#11393);
#11315=PRODUCT_DEFINITION_FORMATION('',$,#11394);
#11316=PRODUCT_DEFINITION_FORMATION('',$,#11395);
#11317=PRODUCT_DEFINITION_FORMATION('',$,#11396);
#11318=PRODUCT_DEFINITION_FORMATION('',$,#11397);
#11319=PRODUCT_DEFINITION_FORMATION('',$,#11398);
#11320=PRODUCT_DEFINITION_FORMATION('',$,#11399);
#11321=PRODUCT_DEFINITION_FORMATION('',$,#11400);
#11322=PRODUCT_DEFINITION_FORMATION('',$,#11401);
#11323=PRODUCT_DEFINITION_FORMATION('',$,#11402);
#11324=PRODUCT_DEFINITION_FORMATION('',$,#11403);
#11325=PRODUCT_DEFINITION_FORMATION('',$,#11404);
#11326=PRODUCT_DEFINITION_FORMATION('',$,#11405);
#11327=PRODUCT_DEFINITION_FORMATION('',$,#11406);
#11328=PRODUCT_DEFINITION_FORMATION('',$,#11407);
#11329=PRODUCT_DEFINITION_FORMATION('',$,#11408);
#11330=PRODUCT_DEFINITION_FORMATION('',$,#11409);
#11331=PRODUCT_DEFINITION_FORMATION('',$,#11410);
#11332=PRODUCT_DEFINITION_FORMATION('',$,#11411);
#11333=PRODUCT_DEFINITION_FORMATION('',$,#11412);
#11334=PRODUCT_DEFINITION_FORMATION('',$,#11413);
#11335=PRODUCT_DEFINITION_FORMATION('',$,#11414);
#11336=PRODUCT_DEFINITION_FORMATION('',$,#11415);
#11337=PRODUCT_DEFINITION_FORMATION('',$,#11416);
#11338=PRODUCT_DEFINITION_FORMATION('',$,#11417);
#11339=PRODUCT_DEFINITION_FORMATION('',$,#11418);
#11340=PRODUCT_DEFINITION_FORMATION('',$,#11419);
#11341=PRODUCT_DEFINITION_FORMATION('',$,#11420);
#11342=PRODUCT_DEFINITION_FORMATION('',$,#11421);
#11343=PRODUCT_DEFINITION_FORMATION('',$,#11422);
#11344=PRODUCT_RELATED_PRODUCT_CATEGORY(
'MAT-063','MAT-063',
(#11385));
#11345=PRODUCT_RELATED_PRODUCT_CATEGORY('Pulley Wheel 1',
'Pulley Wheel 1',(#11386));
#11346=PRODUCT_RELATED_PRODUCT_CATEGORY('Radial Ball Bearing 1',
'Radial Ball Bearing 1',(#11387));
#11347=PRODUCT_RELATED_PRODUCT_CATEGORY('Radial Ball Bearing 2',
'Radial Ball Bearing 2',(#11388));
#11348=PRODUCT_RELATED_PRODUCT_CATEGORY('Pulley Wheel 2',
'Pulley Wheel 2',(#11389));
#11349=PRODUCT_RELATED_PRODUCT_CATEGORY('Belt','Belt',(#11390));
#11350=PRODUCT_RELATED_PRODUCT_CATEGORY('Wheel Support','Wheel Support',
(#11391));
#11351=PRODUCT_RELATED_PRODUCT_CATEGORY('Radial Ball Bearing 3',
'Radial Ball Bearing 3',(#11392));
#11352=PRODUCT_RELATED_PRODUCT_CATEGORY('Mirror Front Support',
'Mirror Front Support',(#11393));
#11353=PRODUCT_RELATED_PRODUCT_CATEGORY('Radial Ball Bearing 4',
'Radial Ball Bearing 4',(#11394));
#11354=PRODUCT_RELATED_PRODUCT_CATEGORY('Broom Roller Assembly',
'Broom Roller Assembly',(#11395));
#11355=PRODUCT_RELATED_PRODUCT_CATEGORY('Broom Roller 1',
'Broom Roller 1',(#11396));
#11356=PRODUCT_RELATED_PRODUCT_CATEGORY('Broom Roller 2',
'Broom Roller 2',(#11397));
#11357=PRODUCT_RELATED_PRODUCT_CATEGORY('Broom Roller 3',
'Broom Roller 3',(#11398));
#11358=PRODUCT_RELATED_PRODUCT_CATEGORY('Broom Roller 4',
'Broom Roller 4',(#11399));
#11359=PRODUCT_RELATED_PRODUCT_CATEGORY('Broom Roller 5',
'Broom Roller 5',(#11400));
#11360=PRODUCT_RELATED_PRODUCT_CATEGORY('Broom Roller 6',
'Broom Roller 6',(#11401));
#11361=PRODUCT_RELATED_PRODUCT_CATEGORY('Broom Roller 7',
'Broom Roller 7',(#11402));
#11362=PRODUCT_RELATED_PRODUCT_CATEGORY('Body','Body',(#11403));
#11363=PRODUCT_RELATED_PRODUCT_CATEGORY('Ground Roller','Ground Roller',
(#11404));
#11364=PRODUCT_RELATED_PRODUCT_CATEGORY('Plate Assembly',
'Plate Assembly',(#11405));
#11365=PRODUCT_RELATED_PRODUCT_CATEGORY('Plate 1','Plate 1',(#11406));
#11366=PRODUCT_RELATED_PRODUCT_CATEGORY('Plate 2','Plate 2',(#11407));
#11367=PRODUCT_RELATED_PRODUCT_CATEGORY('Plate 3','Plate 3',(#11408));
#11368=PRODUCT_RELATED_PRODUCT_CATEGORY('Plate 4','Plate 4',(#11409));
#11369=PRODUCT_RELATED_PRODUCT_CATEGORY('Plate 5','Plate 5',(#11410));
#11370=PRODUCT_RELATED_PRODUCT_CATEGORY('Plate 6','Plate 6',(#11411));
#11371=PRODUCT_RELATED_PRODUCT_CATEGORY('Push Handle Assembly',
'Push Handle Assembly',(#11412));
#11372=PRODUCT_RELATED_PRODUCT_CATEGORY('Push Handle 1','Push Handle 1',
(#11413));
#11373=PRODUCT_RELATED_PRODUCT_CATEGORY('Push Handle 2','Push Handle 2',
(#11414));
#11374=PRODUCT_RELATED_PRODUCT_CATEGORY('Push Handle 3','Push Handle 3',
(#11415));
#11375=PRODUCT_RELATED_PRODUCT_CATEGORY('Push Handle 4','Push Handle 4',
(#11416));
#11376=PRODUCT_RELATED_PRODUCT_CATEGORY('Push Handle 5','Push Handle 5',
(#11417));
#11377=PRODUCT_RELATED_PRODUCT_CATEGORY('Front Support','Front Support',
(#11418));
#11378=PRODUCT_RELATED_PRODUCT_CATEGORY('Wheel Assembly',
'Wheel Assembly',(#11419));
#11379=PRODUCT_RELATED_PRODUCT_CATEGORY('Wheel 1','Wheel 1',(#11420));
#11380=PRODUCT_RELATED_PRODUCT_CATEGORY('Wheel 2','Wheel 2',(#11421));
#11381=PRODUCT_RELATED_PRODUCT_CATEGORY('Wheel 3','Wheel 3',(#11422));
#11382=APPLICATION_PROTOCOL_DEFINITION('international standard',
'automotive_design',2009,#11383);
#11383=APPLICATION_CONTEXT(
'Core Data for Automotive Mechanical Design Process');
#11384=PRODUCT_CONTEXT('part definition',#11383,'mechanical');
#11385=PRODUCT('MAT-063',
'MAT-063',
'LEGAL AND USAGE DISCLAIMER: this Data/Model is provided \X2\201C\X0\A
S IS\X2\201D\X0\ for informational and representational only. It is a 
geometric approximation and is NOT engineered, certified, or guarantee
d for dimensional accuracy, exact tolerances, or production-level prec
ision. Vendor disclaims all implied warranties including fitness for a
 particular purpose. DO NOT USE FOR DIRECT PHYSICAL MANUFACTURING, AUT
OMATED PRODUCTION, OR SAFETY-CRITICAL SYSTEMS without independent engi
neering verification and resolution of any design discrepancies.',(#11384));
#11386=PRODUCT('Pulley Wheel 1','Pulley Wheel 1',
'pulleywheel__ DE    11841',(#11384));
#11387=PRODUCT('Radial Ball Bearing 1','Radial Ball Bearing 1',
'radial ball bearing_68_as_AS_ISO 15 RBB - 415 - 6,SI,NC,6_68__ DE    
10847',(#11384));
#11388=PRODUCT('Radial Ball Bearing 2','Radial Ball Bearing 2',
'radial ball bearing_68_as_AS_ISO 15 RBB - 415 - 6,SI,NC,6_68__ DE    
10847',(#11384));
#11389=PRODUCT('Pulley Wheel 2','Pulley Wheel 2',
'pulleywheel__ DE    11841',(#11384));
#11390=PRODUCT('Belt','Belt','Belt1-13__ DE    13309',(#11384));
#11391=PRODUCT('Wheel Support','Wheel Support',
'wheel_sup__ DE    10163',(#11384));
#11392=PRODUCT('Radial Ball Bearing 3','Radial Ball Bearing 3',
'radial ball bearing_68_as_AS_ISO 15 RBB - 415 - 6,SI,NC,6_68__ DE    
10847',(#11384));
#11393=PRODUCT('Mirror Front Support','Mirror Front Support',
'Mirrorfront_sup__ DE     8799',(#11384));
#11394=PRODUCT('Radial Ball Bearing 4','Radial Ball Bearing 4',
'radial ball bearing_68_as_AS_ISO 15 RBB - 415 - 6,SI,NC,6_68__ DE    
10847',(#11384));
#11395=PRODUCT('Broom Roller Assembly','Broom Roller Assembly',
'broom_and_roller <1>',(#11384));
#11396=PRODUCT('Broom Roller 1','Broom Roller 1',
'broom_and_roller__ DE     7425',(#11384));
#11397=PRODUCT('Broom Roller 2','Broom Roller 2',
'broom_and_roller__ DE     6147',(#11384));
#11398=PRODUCT('Broom Roller 3','Broom Roller 3',
'broom_and_roller__ DE     7205',(#11384));
#11399=PRODUCT('Broom Roller 4','Broom Roller 4',
'broom_and_roller__ DE     5607',(#11384));
#11400=PRODUCT('Broom Roller 5','Broom Roller 5',
'broom_and_roller__ DE     6575',(#11384));
#11401=PRODUCT('Broom Roller 6','Broom Roller 6',
'broom_and_roller__ DE     6985',(#11384));
#11402=PRODUCT('Broom Roller 7','Broom Roller 7',
'broom_and_roller__ DE     6017',(#11384));
#11403=PRODUCT('Body','Body',$,(#11384));
#11404=PRODUCT('Ground Roller','Ground Roller',
'ground_roller__ DE     8465',(#11384));
#11405=PRODUCT('Plate Assembly','Plate Assembly','all_plates <1>',(#11384));
#11406=PRODUCT('Plate 1','Plate 1','all_plates__ DE     1939',(#11384));
#11407=PRODUCT('Plate 2','Plate 2','all_plates__ DE     2307',(#11384));
#11408=PRODUCT('Plate 3','Plate 3','all_plates__ DE      811',(#11384));
#11409=PRODUCT('Plate 4','Plate 4','all_plates__ DE       35',(#11384));
#11410=PRODUCT('Plate 5','Plate 5','all_plates__ DE     1563',(#11384));
#11411=PRODUCT('Plate 6','Plate 6','all_plates__ DE     1187',(#11384));
#11412=PRODUCT('Push Handle Assembly','Push Handle Assembly',
'back_push <1>',(#11384));
#11413=PRODUCT('Push Handle 1','Push Handle 1',
'back_push__ DE     2693',(#11384));
#11414=PRODUCT('Push Handle 2','Push Handle 2',
'back_push__ DE     2589',(#11384));
#11415=PRODUCT('Push Handle 3','Push Handle 3',
'back_push__ DE     3061',(#11384));
#11416=PRODUCT('Push Handle 4','Push Handle 4',
'back_push__ DE     2873',(#11384));
#11417=PRODUCT('Push Handle 5','Push Handle 5',
'back_push__ DE     2477',(#11384));
#11418=PRODUCT('Front Support','Front Support',
'front_sup__ DE     7651',(#11384));
#11419=PRODUCT('Wheel Assembly','Wheel Assembly','wheel <1>',(#11384));
#11420=PRODUCT('Wheel 1','Wheel 1','wheel__ DE     9941',(#11384));
#11421=PRODUCT('Wheel 2','Wheel 2','wheel__ DE     9613',(#11384));
#11422=PRODUCT('Wheel 3','Wheel 3','wheel__ DE     9829',(#11384));
#11423=PRESENTATION_STYLE_ASSIGNMENT((#11427));
#11424=PRESENTATION_STYLE_ASSIGNMENT((#11428));
#11425=PRESENTATION_STYLE_ASSIGNMENT((#11429));
#11426=PRESENTATION_STYLE_ASSIGNMENT((#11430));
#11427=SURFACE_STYLE_USAGE(.BOTH.,#11431);
#11428=SURFACE_STYLE_USAGE(.BOTH.,#11432);
#11429=SURFACE_STYLE_USAGE(.BOTH.,#11433);
#11430=SURFACE_STYLE_USAGE(.BOTH.,#11434);
#11431=SURFACE_SIDE_STYLE('',(#11435));
#11432=SURFACE_SIDE_STYLE('',(#11436));
#11433=SURFACE_SIDE_STYLE('',(#11437));
#11434=SURFACE_SIDE_STYLE('',(#11438));
#11435=SURFACE_STYLE_FILL_AREA(#11439);
#11436=SURFACE_STYLE_FILL_AREA(#11440);
#11437=SURFACE_STYLE_FILL_AREA(#11441);
#11438=SURFACE_STYLE_FILL_AREA(#11442);
#11439=FILL_AREA_STYLE('Steel - Satin',(#11443));
#11440=FILL_AREA_STYLE('Opaque(198,193,188)',(#11444));
#11441=FILL_AREA_STYLE('Opaque(255,242,232)',(#11445));
#11442=FILL_AREA_STYLE('Opaque(202,209,238)',(#11446));
#11443=FILL_AREA_STYLE_COLOUR('Steel - Satin',#11447);
#11444=FILL_AREA_STYLE_COLOUR('Opaque(198,193,188)',#11448);
#11445=FILL_AREA_STYLE_COLOUR('Opaque(255,242,232)',#11449);
#11446=FILL_AREA_STYLE_COLOUR('Opaque(202,209,238)',#11450);
#11447=COLOUR_RGB('Steel - Satin',0.627450980392157,0.627450980392157,0.627450980392157);
#11448=COLOUR_RGB('Opaque(198,193,188)',0.776470588235294,0.756862745098039,
0.737254901960784);
#11449=COLOUR_RGB('Opaque(255,242,232)',1.,0.949019607843137,0.909803921568627);
#11450=COLOUR_RGB('Opaque(202,209,238)',0.792156862745098,0.819607843137255,
0.933333333333333);
ENDSEC;
END-ISO-10303-21;
